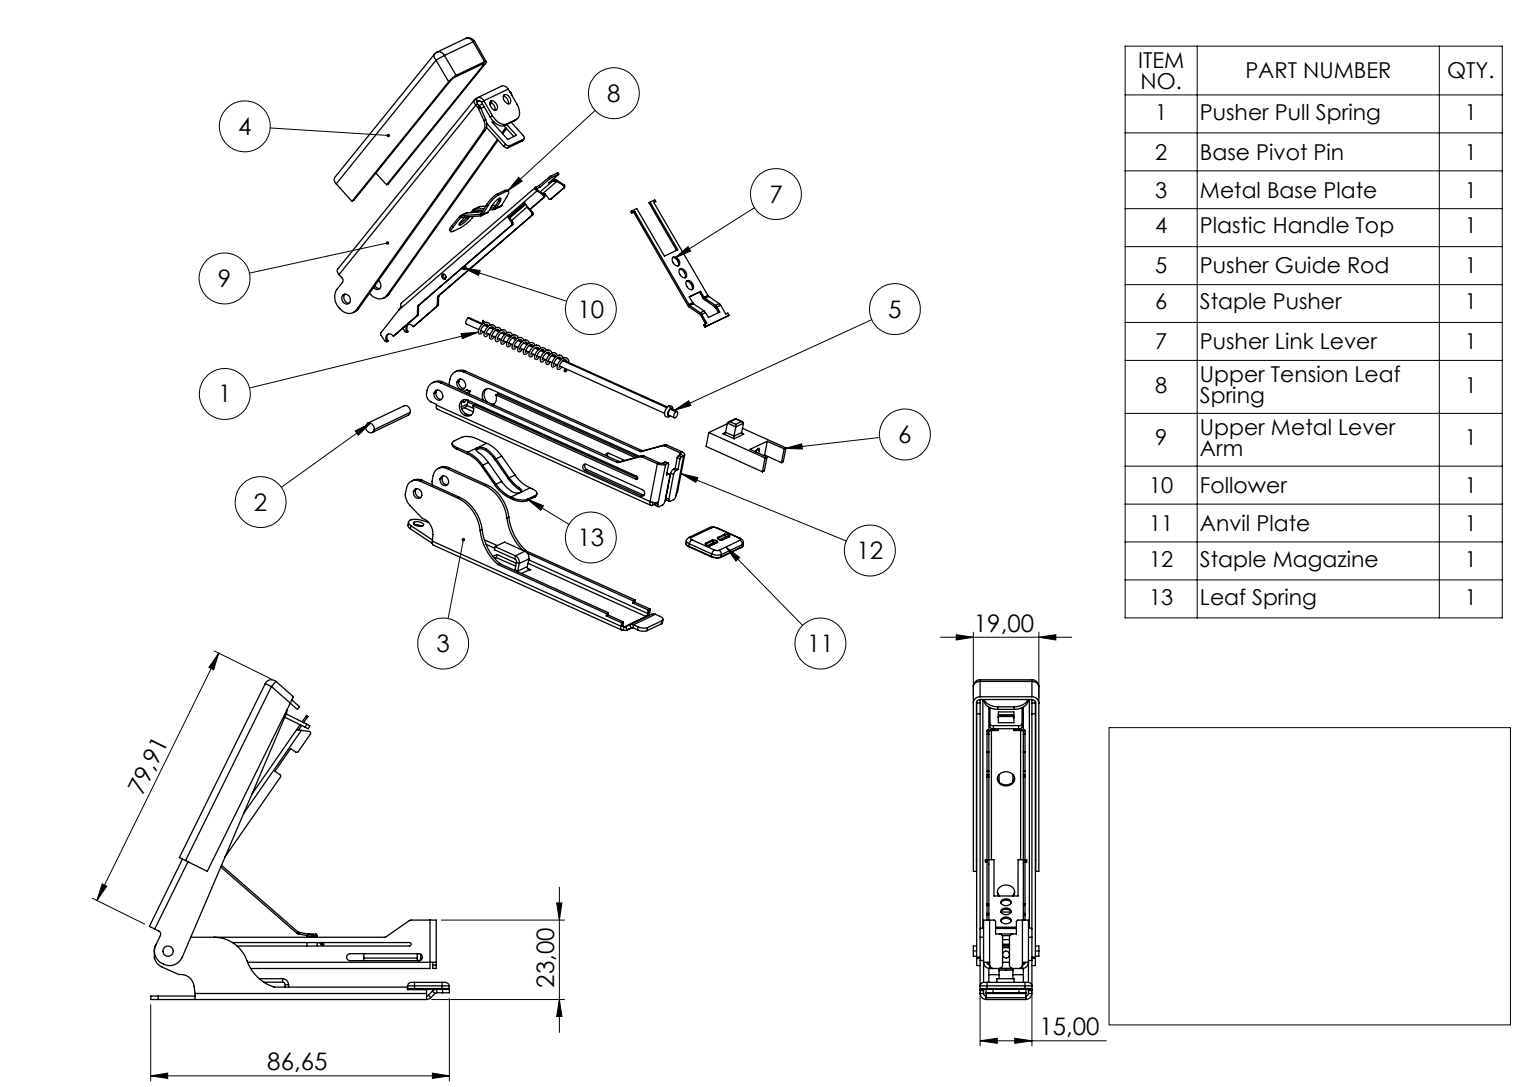
ISO-10303-21;
HEADER;
FILE_DESCRIPTION (('STEP AP214'),
    '1' );
FILE_NAME ('MAS-155',
    '2026-10-06T10:23:46',
    ( '' ),
    ( '' ),
    'SwSTEP 2.0',
    'SolidWorks 2020',
    '' );
FILE_SCHEMA (( 'AUTOMOTIVE_DESIGN' ));
ENDSEC;

DATA;
#1 = CARTESIAN_POINT ( 'NONE',  ( 35.64099152588522657, -0.6071811381869983704, 82.55501292736997243 ) ) ;
#2 = ORIENTED_EDGE ( 'NONE', *, *, #5924, .T. ) ;
#3 = DIRECTION ( 'NONE',  ( -2.412663730047099099E-15, 0.8967398287344627850, 0.4425581086832399147 ) ) ;
#4 = CARTESIAN_POINT ( 'NONE',  ( 32.56606138205700773, 43.35512946304240245, 83.12823623207320622 ) ) ;
#5 = CARTESIAN_POINT ( 'NONE',  ( 39.02088643472237806, -8.703840866421918676, 73.73360434286902887 ) ) ;
#6 = DIRECTION ( 'NONE',  ( 0.000000000000000000, 0.9992330079037401447, -0.03915859951075795903 ) ) ;
#7 = CARTESIAN_POINT ( 'NONE',  ( 38.82593461698262871, -16.91368208888610170, 69.62690120949091011 ) ) ;
#8 = FACE_OUTER_BOUND ( 'NONE', #24823, .T. ) ;
#9 = CARTESIAN_POINT ( 'NONE',  ( 37.25202387243752611, -25.21368208888610241, 70.00779233799262613 ) ) ;
#10 = VECTOR ( 'NONE', #20731, 1000.000000000000000 ) ;
#11 = DIRECTION ( 'NONE',  ( -6.056754644426120895E-31, -1.000000000000000000, -4.914813388431354887E-16 ) ) ;
#12 = CARTESIAN_POINT ( 'NONE',  ( 36.80608444377002542, -2.303840866421914768, 72.40698646996135324 ) ) ;
#13 = EDGE_CURVE ( 'NONE', #2345, #1520, #288, .T. ) ;
#14 = DIRECTION ( 'NONE',  ( 0.000000000000000000, 0.000000000000000000, 1.000000000000000000 ) ) ;
#15 = CARTESIAN_POINT ( 'NONE',  ( 39.82603832034400426, -20.31368208888610738, 72.40698646996133903 ) ) ;
#16 = EDGE_CURVE ( 'NONE', #3263, #15554, #24734, .T. ) ;
#17 = DIRECTION ( 'NONE',  ( -9.925461516413211857E-16, 0.8967398287344598984, 0.4425581086832454658 ) ) ;
#18 = CARTESIAN_POINT ( 'NONE',  ( 36.68196826583682935, -18.00384086642191406, 70.79240656858107172 ) ) ;
#19 = CARTESIAN_POINT ( 'NONE',  ( 35.14099152588522657, 1.392818861812999964, 83.30501292736997243 ) ) ;
#20 = CIRCLE ( 'NONE', #15263, 1.000000000000000888 ) ;
#21 = CARTESIAN_POINT ( 'NONE',  ( 36.64852494920107517, -13.41368208888610525, 70.89533451361947414 ) ) ;
#22 = VERTEX_POINT ( 'NONE', #10978 ) ;
#23 = CARTESIAN_POINT ( 'NONE',  ( 39.12911128074873801, -24.11368208888611164, 73.69843995877326392 ) ) ;
#24 = ORIENTED_EDGE ( 'NONE', *, *, #17686, .T. ) ;
#25 = DIRECTION ( 'NONE',  ( 8.673617379884039170E-17, 2.999999999999999839E-15, 1.000000000000000000 ) ) ;
#26 = DIRECTION ( 'NONE',  ( 1.327674326049719602E-15, -0.4425581086832399147, 0.8967398287344627850 ) ) ;
#27 = CIRCLE ( 'NONE', #15267, 0.2000000000000057288 ) ;
#28 = CARTESIAN_POINT ( 'NONE',  ( 38.26194895904384197, -26.60384086642191193, 72.51602215082114355 ) ) ;
#29 = EDGE_LOOP ( 'NONE', ( #453, #19107 ) ) ;
#30 = VERTEX_POINT ( 'NONE', #22566 ) ;
#31 = LINE ( 'NONE', #9973, #22803 ) ;
#32 = EDGE_CURVE ( 'NONE', #20252, #1331, #16766, .T. ) ;
#33 = CARTESIAN_POINT ( 'NONE',  ( 40.81606138205700773, -31.05876147765399864, 75.30501292737010033 ) ) ;
#34 = ORIENTED_EDGE ( 'NONE', *, *, #8349, .T. ) ;
#35 = DIRECTION ( 'NONE',  ( -1.000000000000000000, -3.091505625455828697E-15, -4.515976121274772923E-17 ) ) ;
#36 = CARTESIAN_POINT ( 'NONE',  ( 36.29569395875881099, -26.30384086642192187, 72.77780686321126780 ) ) ;
#37 = CARTESIAN_POINT ( 'NONE',  ( 33.31606138205700773, -26.06829118875199569, 75.80501292736998664 ) ) ;
#38 = CARTESIAN_POINT ( 'NONE',  ( 36.89935272106204422, -5.213682088886100630, 69.52238214136768590 ) ) ;
#39 = B_SPLINE_SURFACE_WITH_KNOTS ( 'NONE', 1, 3, ( 
 ( #3682, #6010, #7951, #7688 ),
 ( #11564, #15795, #4076, #7569 ) ),
 .UNSPECIFIED., .F., .F., .F.,
 ( 2, 2 ),
 ( 4, 4 ),
 ( 0.000000000000000000, 1.000000000000000000 ),
 ( 0.000000000000000000, 1.000000000000000000 ),
 .UNSPECIFIED. ) ;
#40 = CARTESIAN_POINT ( 'NONE',  ( 42.06606138205700063, 43.19123852234599781, 75.30501292736987295 ) ) ;
#41 = ORIENTED_EDGE ( 'NONE', *, *, #9883, .F. ) ;
#42 = ORIENTED_EDGE ( 'NONE', *, *, #4052, .T. ) ;
#43 = CARTESIAN_POINT ( 'NONE',  ( 33.24020206407681144, 3.104049617356281932, 6.135536031321588091 ) ) ;
#44 = CARTESIAN_POINT ( 'NONE',  ( 38.37017380507020192, 1.986317911113890444, 73.11602215082119471 ) ) ;
#45 = CARTESIAN_POINT ( 'NONE',  ( 36.80608444377002542, -24.30384086642191832, 72.40698646996131060 ) ) ;
#46 =( NAMED_UNIT ( * ) SI_UNIT ( $, .STERADIAN. ) SOLID_ANGLE_UNIT ( ) );
#47 = DIRECTION ( 'NONE',  ( 0.000000000000000000, 0.000000000000000000, -1.000000000000000000 ) ) ;
#48 = AXIS2_PLACEMENT_3D ( 'NONE', #18248, #195, #19789 ) ;
#49 = EDGE_LOOP ( 'NONE', ( #5787, #14617, #11097, #246 ) ) ;
#50 = DIRECTION ( 'NONE',  ( 1.000000000000000000, 2.751104698760144965E-15, -1.228345504986737969E-16 ) ) ;
#51 = VECTOR ( 'NONE', #12391, 1000.000000000000227 ) ;
#52 = CARTESIAN_POINT ( 'NONE',  ( 38.31606138205700773, -22.27515649656512053, 29.48506754039017963 ) ) ;
#53 = ORIENTED_EDGE ( 'NONE', *, *, #21241, .F. ) ;
#54 = CARTESIAN_POINT ( 'NONE',  ( 39.51027997493896748, -3.103840866421909706, 71.43714994484034264 ) ) ;
#55 = LINE ( 'NONE', #13982, #12355 ) ;
#56 = ORIENTED_EDGE ( 'NONE', *, *, #3919, .F. ) ;
#57 = DIRECTION ( 'NONE',  ( 0.000000000000000000, 1.000000000000000000, -3.469446951953613400E-15 ) ) ;
#58 = VERTEX_POINT ( 'NONE', #8676 ) ;
#59 = VERTEX_POINT ( 'NONE', #24601 ) ;
#60 = CARTESIAN_POINT ( 'NONE',  ( 41.31606138205700063, 9.119667998728431257, 66.98393923633439329 ) ) ;
#61 = CARTESIAN_POINT ( 'NONE',  ( 39.31564783533280405, -12.31368208888610027, 72.03616607671141026 ) ) ;
#62 = CARTESIAN_POINT ( 'NONE',  ( 39.51027997493896748, -10.51368208888610134, 71.32335560751961623 ) ) ;
#63 = ORIENTED_EDGE ( 'NONE', *, *, #7607, .F. ) ;
#64 = VERTEX_POINT ( 'NONE', #911 ) ;
#65 = DIRECTION ( 'NONE',  ( 0.000000000000000000, 1.000000000000000000, -2.775557561562891351E-15 ) ) ;
#66 = EDGE_CURVE ( 'NONE', #3119, #2388, #6890, .T. ) ;
#67 = CARTESIAN_POINT ( 'NONE',  ( 33.31606138205700773, -20.55619265724211076, 44.11584019928223910 ) ) ;
#68 = EDGE_LOOP ( 'NONE', ( #6538, #19929, #5268, #8723 ) ) ;
#69 = FACE_OUTER_BOUND ( 'NONE', #11931, .T. ) ;
#70 = CARTESIAN_POINT ( 'NONE',  ( 39.29254315202757653, -18.80384086642191477, 72.81632618279321889 ) ) ;
#71 = VECTOR ( 'NONE', #6423, 1000.000000000000227 ) ;
#72 = LINE ( 'NONE', #4208, #11613 ) ;
#73 = AXIS2_PLACEMENT_3D ( 'NONE', #20617, #20868, #18556 ) ;
#74 = DIRECTION ( 'NONE',  ( 0.000000000000000000, -0.5735764363510444941, 0.8191520442889929088 ) ) ;
#75 = CARTESIAN_POINT ( 'NONE',  ( 38.37017380507020192, -18.01368208888610312, 72.51602215082118619 ) ) ;
#76 = ORIENTED_EDGE ( 'NONE', *, *, #14029, .F. ) ;
#77 = ORIENTED_EDGE ( 'NONE', *, *, #24683, .F. ) ;
#78 = FACE_BOUND ( 'NONE', #23310, .T. ) ;
#79 = CARTESIAN_POINT ( 'NONE',  ( 37.33957961208646736, -13.81368208888610916, 72.81632618279321889 ) ) ;
#80 = CARTESIAN_POINT ( 'NONE',  ( 44.81606138205700063, -25.52563857111379875, 92.39878177866870601 ) ) ;
#81 = CARTESIAN_POINT ( 'NONE',  ( 43.81606138205700063, -33.39268736607245103, 60.15578379404454523 ) ) ;
#82 = CARTESIAN_POINT ( 'NONE',  ( 39.82603832034400426, -28.31368208888610027, 72.40698646996131060 ) ) ;
#83 = CARTESIAN_POINT ( 'NONE',  ( 40.08931077638955998, -29.10876147764802369, 70.44264307849509521 ) ) ;
#84 = CIRCLE ( 'NONE', #17364, 0.7500000000000006661 ) ;
#85 = CARTESIAN_POINT ( 'NONE',  ( 33.31606138205700773, -20.55619265724211076, 44.11584019928223910 ) ) ;
#86 = ORIENTED_EDGE ( 'NONE', *, *, #3104, .F. ) ;
#87 = VECTOR ( 'NONE', #691, 1000.000000000000114 ) ;
#88 = CARTESIAN_POINT ( 'NONE',  ( 33.31606138205700773, 7.043113989679085307, 66.83274420321491505 ) ) ;
#89 = EDGE_LOOP ( 'NONE', ( #3243, #17530, #4061, #10924 ) ) ;
#90 = ORIENTED_EDGE ( 'NONE', *, *, #479, .T. ) ;
#91 = CARTESIAN_POINT ( 'NONE',  ( 39.73277004305197124, -5.403840866421909972, 69.52238214136768590 ) ) ;
#92 = ORIENTED_EDGE ( 'NONE', *, *, #24380, .T. ) ;
#93 = AXIS2_PLACEMENT_3D ( 'NONE', #14032, #16324, #20207 ) ;
#94 = EDGE_CURVE ( 'NONE', #4444, #1424, #20510, .T. ) ;
#95 = DIRECTION ( 'NONE',  ( 1.000000000000000000, 0.000000000000000000, 0.000000000000000000 ) ) ;
#96 = CARTESIAN_POINT ( 'NONE',  ( 39.95015449827720744, -8.613682088886104538, 70.79240656858107172 ) ) ;
#97 = EDGE_LOOP ( 'NONE', ( #25397, #5551, #19425, #6383 ) ) ;
#98 = CARTESIAN_POINT ( 'NONE',  ( 29.81606138205697221, -3.227578639999851617, -4.500312080287595329 ) ) ;
#99 = CARTESIAN_POINT ( 'NONE',  ( 40.33642880535524000, -12.31368208888611093, 72.77780686321126780 ) ) ;
#100 = DIRECTION ( 'NONE',  ( 0.000000000000000000, -0.5706330172266907974, 0.8212051873014217795 ) ) ;
#101 = CARTESIAN_POINT ( 'NONE',  ( 35.64099152588522657, 40.83281886181300280, 79.30501292736983032 ) ) ;
#102 = AXIS2_PLACEMENT_3D ( 'NONE', #15158, #5376, #18644 ) ;
#103 = DIRECTION ( 'NONE',  ( 2.312964634635740294E-15, 2.999999999999999839E-15, 1.000000000000000000 ) ) ;
#104 = ADVANCED_FACE ( 'NONE', ( #4789 ), #24864, .T. ) ;
#105 =( NAMED_UNIT ( * ) PLANE_ANGLE_UNIT ( ) SI_UNIT ( $, .RADIAN. ) );
#106 = ADVANCED_FACE ( 'NONE', ( #10603 ), #18707, .F. ) ;
#107 = LINE ( 'NONE', #13782, #2826 ) ;
#108 = VECTOR ( 'NONE', #19668, 1000.000000000000000 ) ;
#109 = EDGE_CURVE ( 'NONE', #2100, #16742, #24351, .T. ) ;
#110 = LINE ( 'NONE', #17914, #18667 ) ;
#111 = EDGE_CURVE ( 'NONE', #24693, #6631, #6848, .T. ) ;
#112 = CARTESIAN_POINT ( 'NONE',  ( 37.69225076346193504, -15.80384086642191299, 70.42958956619168021 ) ) ;
#113 = CARTESIAN_POINT ( 'NONE',  ( 39.37952058850012804, -22.61368208888610454, 70.97781676520601479 ) ) ;
#114 = EDGE_CURVE ( 'NONE', #23891, #14933, #22516, .T. ) ;
#115 = ORIENTED_EDGE ( 'NONE', *, *, #16759, .F. ) ;
#116 = CARTESIAN_POINT ( 'NONE',  ( 44.81606138205700063, -24.55876147765401285, 70.30501292737008612 ) ) ;
#117 = VECTOR ( 'NONE', #18081, 1000.000000000000000 ) ;
#118 = CYLINDRICAL_SURFACE ( 'NONE', #9476, 1.000000000000000888 ) ;
#119 = ORIENTED_EDGE ( 'NONE', *, *, #11030, .T. ) ;
#120 = VERTEX_POINT ( 'NONE', #3105 ) ;
#121 = CARTESIAN_POINT ( 'NONE',  ( 38.26194895904384197, -22.60384086642191903, 73.71602215082113219 ) ) ;
#122 = AXIS2_PLACEMENT_3D ( 'NONE', #22603, #19127, #1077 ) ;
#123 = ADVANCED_FACE ( 'NONE', ( #785 ), #7110, .F. ) ;
#124 = CARTESIAN_POINT ( 'NONE',  ( 37.12184278917507640, -23.51368208888609956, 71.43714994484032843 ) ) ;
#125 = CARTESIAN_POINT ( 'NONE',  ( 37.61123632939165873, -5.913682088886105248, 73.73360434286902887 ) ) ;
#126 = VERTEX_POINT ( 'NONE', #6729 ) ;
#127 = DIRECTION ( 'NONE',  ( 0.000000000000000000, 1.000000000000000000, -2.775557561562891351E-15 ) ) ;
#128 = EDGE_CURVE ( 'NONE', #1147, #21871, #2352, .T. ) ;
#129 = CARTESIAN_POINT ( 'NONE',  ( 37.25260217561390874, -0.003840866421911393481, 70.97781676520604321 ) ) ;
#130 = FACE_OUTER_BOUND ( 'NONE', #3742, .T. ) ;
#131 = VERTEX_POINT ( 'NONE', #14581 ) ;
#132 = AXIS2_PLACEMENT_3D ( 'NONE', #6490, #16519, #18844 ) ;
#133 = CARTESIAN_POINT ( 'NONE',  ( 40.64099152588522657, -1.357181138186998925, 80.05501292737000085 ) ) ;
#134 = DIRECTION ( 'NONE',  ( 0.000000000000000000, -0.8212051873014223347, -0.5706330172266899092 ) ) ;
#135 = CARTESIAN_POINT ( 'NONE',  ( 36.89935272106205133, -6.403840866421917077, 73.23812341099225875 ) ) ;
#136 = FACE_OUTER_BOUND ( 'NONE', #6898, .T. ) ;
#137 = SURFACE_STYLE_USAGE ( .BOTH. , #13306 ) ;
#138 = MECHANICAL_DESIGN_GEOMETRIC_PRESENTATION_REPRESENTATION (  '', ( #5078 ), #1784 ) ;
#139 = CARTESIAN_POINT ( 'NONE',  ( 39.95015449827720744, -12.61368208888610454, 70.79240656858105751 ) ) ;
#140 = CARTESIAN_POINT ( 'NONE',  ( 33.63257508155574271, 2.837830513113388076, 6.099065269017614810 ) ) ;
#141 = EDGE_CURVE ( 'NONE', #14226, #13391, #3231, .T. ) ;
#142 = CARTESIAN_POINT ( 'NONE',  ( 36.87297107704153376, -25.71368208888610596, 72.49904802271738902 ) ) ;
#143 = VECTOR ( 'NONE', #19074, 1000.000000000000000 ) ;
#144 = LINE ( 'NONE', #15861, #20989 ) ;
#145 = CIRCLE ( 'NONE', #6320, 1.000000000000000888 ) ;
#146 = CARTESIAN_POINT ( 'NONE',  ( 36.87297107704151244, -1.903840866421906641, 70.26145752964255564 ) ) ;
#147 = CARTESIAN_POINT ( 'NONE',  ( 38.48938833801555148, 40.69123852234599781, 72.28987726642291989 ) ) ;
#148 = CARTESIAN_POINT ( 'NONE',  ( 36.80608444377001121, -19.31368208888609672, 70.35351908239857721 ) ) ;
#149 = DIRECTION ( 'NONE',  ( 0.000000000000000000, -0.7540134720837687876, -0.6568589528324780824 ) ) ;
#150 = AXIS2_PLACEMENT_3D ( 'NONE', #11257, #7991, #1314 ) ;
#151 = CARTESIAN_POINT ( 'NONE',  ( 39.38009889167648936, -17.40384086642190908, 70.00779233799262613 ) ) ;
#152 = LINE ( 'NONE', #3900, #22918 ) ;
#153 = CARTESIAN_POINT ( 'NONE',  ( 36.64852494920107517, -11.41368208888610525, 70.89533451361947414 ) ) ;
#154 = VERTEX_POINT ( 'NONE', #12549 ) ;
#155 = CARTESIAN_POINT ( 'NONE',  ( 37.50301148336529167, -19.11368208888609388, 69.06206559358665231 ) ) ;
#156 = ORIENTED_EDGE ( 'NONE', *, *, #18156, .F. ) ;
#157 = CARTESIAN_POINT ( 'NONE',  ( 36.31606138205700063, 39.69123852234597649, 69.30501292736988717 ) ) ;
#158 = AXIS2_PLACEMENT_3D ( 'NONE', #16213, #10429, #24064 ) ;
#159 = CARTESIAN_POINT ( 'NONE',  ( 41.31606138205700063, 7.187001342539796944, 66.09667597968754649 ) ) ;
#160 = CARTESIAN_POINT ( 'NONE',  ( 38.73920764526923932, -19.50384086642191406, 70.26206559358661252 ) ) ;
#161 = ORIENTED_EDGE ( 'NONE', *, *, #12871, .T. ) ;
#162 = ORIENTED_EDGE ( 'NONE', *, *, #2908, .T. ) ;
#163 = CARTESIAN_POINT ( 'NONE',  ( 39.59824383043523000, -28.76838690529542220, 70.55371702292011094 ) ) ;
#164 = CIRCLE ( 'NONE', #21962, 1.000000000000000888 ) ;
#165 = LINE ( 'NONE', #13580, #21925 ) ;
#166 = CARTESIAN_POINT ( 'NONE',  ( 40.26954217208372455, -20.90384086642191974, 72.86986841596734621 ) ) ;
#167 = CARTESIAN_POINT ( 'NONE',  ( 36.07789103942398867, 0.5863179111138955291, 70.70992431699450265 ) ) ;
#168 = DIRECTION ( 'NONE',  ( 0.000000000000000000, 1.000000000000000000, -3.469446951953613400E-15 ) ) ;
#169 = ORIENTED_EDGE ( 'NONE', *, *, #3276, .T. ) ;
#170 = VERTEX_POINT ( 'NONE', #12668 ) ;
#171 = CARTESIAN_POINT ( 'NONE',  ( 43.31606138205700063, 3.536347952325769040, 64.10938348997790115 ) ) ;
#172 =( GEOMETRIC_REPRESENTATION_CONTEXT ( 3 ) GLOBAL_UNCERTAINTY_ASSIGNED_CONTEXT ( ( #8249 ) ) GLOBAL_UNIT_ASSIGNED_CONTEXT ( ( #2358, #16143, #22073 ) ) REPRESENTATION_CONTEXT ( 'NONE', 'WORKASPACE' ) );
#173 = DIRECTION ( 'NONE',  ( 0.000000000000000000, 1.000000000000000000, -3.469446951953701358E-15 ) ) ;
#174 = CARTESIAN_POINT ( 'NONE',  ( 36.68196826583682935, -24.00384086642191050, 70.79240656858105751 ) ) ;
#175 = FILL_AREA_STYLE ('',( #23869 ) ) ;
#176 = DIRECTION ( 'NONE',  ( 0.000000000000000000, 0.9814242980364923374, 0.1918498038142812112 ) ) ;
#177 = ORIENTED_EDGE ( 'NONE', *, *, #13046, .F. ) ;
#178 = LINE ( 'NONE', #16145, #1575 ) ;
#179 = DIRECTION ( 'NONE',  ( 1.000000000000000000, -5.204170427930413997E-31, -1.734723475976804876E-16 ) ) ;
#180 = VERTEX_POINT ( 'NONE', #7626 ) ;
#181 = CARTESIAN_POINT ( 'NONE',  ( 39.41296390513587511, -9.203840866421909794, 71.08074471024443142 ) ) ;
#182 = CARTESIAN_POINT ( 'NONE',  ( 42.90896497783001706, 3.030042170879425178, 6.235548050178295831 ) ) ;
#183 = ORIENTED_EDGE ( 'NONE', *, *, #6628, .F. ) ;
#184 = CARTESIAN_POINT ( 'NONE',  ( 31.91606138205697718, -5.022037326221728826, -5.474317061061731771 ) ) ;
#185 = ORIENTED_EDGE ( 'NONE', *, *, #16638, .F. ) ;
#186 = ORIENTED_EDGE ( 'NONE', *, *, #12634, .T. ) ;
#187 = CARTESIAN_POINT ( 'NONE',  ( 43.23147868389327897, 41.90149715599300606, 79.87823623207322044 ) ) ;
#188 = CARTESIAN_POINT ( 'NONE',  ( 39.31564783533280405, -6.313682088886101162, 72.03616607671141026 ) ) ;
#189 = CARTESIAN_POINT ( 'NONE',  ( 39.02742774030102879, -4.213682088886099741, 72.26730301774236409 ) ) ;
#190 = ORIENTED_EDGE ( 'NONE', *, *, #18404, .F. ) ;
#191 = EDGE_LOOP ( 'NONE', ( #11726, #12081, #22272, #24674 ) ) ;
#192 = DIRECTION ( 'NONE',  ( 0.000000000000000000, 1.000000000000000000, -3.469446951953613400E-15 ) ) ;
#193 = DIRECTION ( 'NONE',  ( -1.927470528863119788E-16, -1.000000000000000000, 2.999999999999999839E-15 ) ) ;
#194 = VERTEX_POINT ( 'NONE', #1 ) ;
#195 = DIRECTION ( 'NONE',  ( 1.000000000000000000, -0.000000000000000000, 0.000000000000000000 ) ) ;
#196 = CARTESIAN_POINT ( 'NONE',  ( 38.93415946300896024, -17.50384086642190695, 69.66206559358661821 ) ) ;
#197 = VECTOR ( 'NONE', #7883, 1000.000000000000000 ) ;
#198 = EDGE_CURVE ( 'NONE', #24709, #13605, #5816, .T. ) ;
#199 = EDGE_CURVE ( 'NONE', #8460, #24765, #19336, .T. ) ;
#200 = CARTESIAN_POINT ( 'NONE',  ( 37.42719827050449055, -22.02795882147844964, 75.81186121921504650 ) ) ;
#201 = CARTESIAN_POINT ( 'NONE',  ( 44.81606138205700063, 41.44123852234595518, 61.30501292736988006 ) ) ;
#202 = CARTESIAN_POINT ( 'NONE',  ( 44.81606138205700063, 40.34464305740947765, 81.44836866983821722 ) ) ;
#203 = VERTEX_POINT ( 'NONE', #23192 ) ;
#204 = ORIENTED_EDGE ( 'NONE', *, *, #17940, .F. ) ;
#205 = LINE ( 'NONE', #24148, #14945 ) ;
#206 = CARTESIAN_POINT ( 'NONE',  ( 39.82603832034401847, -12.31368208888610738, 72.40698646996131060 ) ) ;
#207 = CARTESIAN_POINT ( 'NONE',  ( 40.31606138205700773, 37.94123852234599070, 73.55501292736988717 ) ) ;
#208 = LINE ( 'NONE', #4092, #1342 ) ;
#209 = LINE ( 'NONE', #23668, #17662 ) ;
#210 = LINE ( 'NONE', #8213, #17640 ) ;
#211 = ADVANCED_FACE ( 'NONE', ( #19460 ), #5431, .T. ) ;
#212 = VECTOR ( 'NONE', #20996, 1000.000000000000000 ) ;
#213 = AXIS2_PLACEMENT_3D ( 'NONE', #12528, #8134, #2696 ) ;
#214 = CARTESIAN_POINT ( 'NONE',  ( 33.31606138205700773, -14.32738121993777192, 11.12118157620986558 ) ) ;
#215 = LINE ( 'NONE', #15932, #731 ) ;
#216 = EDGE_LOOP ( 'NONE', ( #18034, #25103, #6817, #21837 ) ) ;
#217 = CARTESIAN_POINT ( 'NONE',  ( 31.81606138205700418, -31.45856502260510013, 77.07494475056050476 ) ) ;
#218 = EDGE_LOOP ( 'NONE', ( #9842, #8008, #1464, #22702 ) ) ;
#219 = ORIENTED_EDGE ( 'NONE', *, *, #5616, .T. ) ;
#220 = CARTESIAN_POINT ( 'NONE',  ( 36.11133435605973574, -6.003840866421917610, 70.60699637195612866 ) ) ;
#221 = ORIENTED_EDGE ( 'NONE', *, *, #10919, .F. ) ;
#222 = DIRECTION ( 'NONE',  ( 0.000000000000000000, -2.999999999999999839E-15, -1.000000000000000000 ) ) ;
#223 = CARTESIAN_POINT ( 'NONE',  ( 37.80618814713140097, -9.913682088886107024, 73.13360434286904876 ) ) ;
#224 = ORIENTED_EDGE ( 'NONE', *, *, #10845, .T. ) ;
#225 = CARTESIAN_POINT ( 'NONE',  ( 30.81606138205700418, -21.15876147765410309, 66.30501292737000085 ) ) ;
#226 = CARTESIAN_POINT ( 'NONE',  ( 36.29569395875879678, -15.31368208888610205, 69.98269868914867686 ) ) ;
#227 = DIRECTION ( 'NONE',  ( -1.000000000000000000, -2.999999999999999839E-15, 0.000000000000000000 ) ) ;
#228 = CARTESIAN_POINT ( 'NONE',  ( 32.81606138205700773, 36.92314894770294131, 81.17823623207323180 ) ) ;
#229 = CYLINDRICAL_SURFACE ( 'NONE', #16961, 0.5000000000000004441 ) ;
#230 = DIRECTION ( 'NONE',  ( 1.000000000000000000, 1.518641380243644581E-16, 1.055262346480601087E-16 ) ) ;
#231 = EDGE_CURVE ( 'NONE', #16465, #14577, #22942, .T. ) ;
#232 = CARTESIAN_POINT ( 'NONE',  ( 32.81606138205700773, -27.11289203277224402, 56.96090842897168471 ) ) ;
#233 = DIRECTION ( 'NONE',  ( -1.849283715844614702E-16, 0.8212051873014210024, 0.5706330172266920187 ) ) ;
#234 = CARTESIAN_POINT ( 'NONE',  ( 38.93987200065208754, -24.81368208888610738, 70.42958956619166599 ) ) ;
#235 = VERTEX_POINT ( 'NONE', #24984 ) ;
#236 = CARTESIAN_POINT ( 'NONE',  ( 40.81606138205700063, 9.191238522346999673, 69.30501292736997243 ) ) ;
#237 = DIRECTION ( 'NONE',  ( 1.000000000000000000, 0.000000000000000000, 0.000000000000000000 ) ) ;
#238 = ORIENTED_EDGE ( 'NONE', *, *, #7921, .F. ) ;
#239 = ORIENTED_EDGE ( 'NONE', *, *, #12746, .F. ) ;
#240 = CARTESIAN_POINT ( 'NONE',  ( 37.61123632939164452, -25.70384086642191690, 69.02690120949091579 ) ) ;
#241 = CARTESIAN_POINT ( 'NONE',  ( 37.33957961208646736, -27.81368208888611093, 72.81632618279320468 ) ) ;
#242 = DIRECTION ( 'NONE',  ( 1.218693434051482139E-16, -0.4425581086832393041, 0.8967398287344630070 ) ) ;
#243 = EDGE_CURVE ( 'NONE', #17020, #9362, #11367, .T. ) ;
#244 = LINE ( 'NONE', #4267, #5670 ) ;
#245 = EDGE_CURVE ( 'NONE', #15791, #17958, #9316, .T. ) ;
#246 = ORIENTED_EDGE ( 'NONE', *, *, #17263, .T. ) ;
#247 = CARTESIAN_POINT ( 'NONE',  ( 39.93368021267864520, -5.986475166052370511, 82.77450256188085120 ) ) ;
#248 = CYLINDRICAL_SURFACE ( 'NONE', #25213, 0.7500000000000006661 ) ;
#249 = CARTESIAN_POINT ( 'NONE',  ( 40.77203464402485622, -1.103840866421915035, 71.43714994484034264 ) ) ;
#250 = EDGE_CURVE ( 'NONE', #6034, #3058, #21270, .T. ) ;
#251 = EDGE_CURVE ( 'NONE', #21293, #8440, #21528, .T. ) ;
#252 = ADVANCED_FACE ( 'NONE', ( #23316 ), #17669, .F. ) ;
#253 = DIRECTION ( 'NONE',  ( 1.000000000000000275E-15, -0.9439899321577401858, -0.3299742535180970604 ) ) ;
#254 = CYLINDRICAL_SURFACE ( 'NONE', #13248, 1.000000000000000888 ) ;
#255 = CARTESIAN_POINT ( 'NONE',  ( 39.95015449827720744, -4.613682088886104538, 70.79240656858107172 ) ) ;
#256 = CARTESIAN_POINT ( 'NONE',  ( 39.29254315202756231, -24.81368208888610383, 69.94417936956671156 ) ) ;
#257 = CARTESIAN_POINT ( 'NONE',  ( 34.56606138205700773, 45.04446929126255128, 81.37823623207320622 ) ) ;
#258 = ADVANCED_FACE ( 'NONE', ( #25369 ), #5308, .T. ) ;
#259 = CARTESIAN_POINT ( 'NONE',  ( 39.98359781491296161, -3.203840866421912903, 70.89533451361947414 ) ) ;
#261 = EDGE_CURVE ( 'NONE', #11274, #17540, #5561, .T. ) ;
#260 = CONTEXT_DEPENDENT_SHAPE_REPRESENTATION ( #7838, #3099 ) ;
#262 = CARTESIAN_POINT ( 'NONE',  ( 32.81606138205700773, 2.191238522347013440, 73.80501292737000085 ) ) ;
#263 = CARTESIAN_POINT ( 'NONE',  ( 37.21915885897815457, -26.20384086642190979, 71.67976084211551324 ) ) ;
#264 = CARTESIAN_POINT ( 'NONE',  ( 36.64852494920107517, -9.413682088886107024, 70.89533451361948835 ) ) ;
#265 = LINE ( 'NONE', #13690, #19298 ) ;
#266 = AXIS2_PLACEMENT_3D ( 'NONE', #24025, #20423, #700 ) ;
#267 = CARTESIAN_POINT ( 'NONE',  ( 36.64852494920107517, -10.20384086642191157, 71.86517103874049894 ) ) ;
#268 = DIRECTION ( 'NONE',  ( 1.000000000000000000, 3.083952846180988900E-15, -3.854941057726327830E-16 ) ) ;
#269 = VECTOR ( 'NONE', #16270, 1000.000000000000000 ) ;
#270 = CIRCLE ( 'NONE', #24538, 2.000000000000001776 ) ;
#271 = CARTESIAN_POINT ( 'NONE',  ( 36.64852494920107517, -9.413682088886107024, 70.89533451361948835 ) ) ;
#272 = ORIENTED_EDGE ( 'NONE', *, *, #16077, .F. ) ;
#273 = CARTESIAN_POINT ( 'NONE',  ( 38.37017380507020192, -18.01368208888610667, 73.71602215082113219 ) ) ;
#274 = EDGE_LOOP ( 'NONE', ( #318, #14239, #23744, #24928 ) ) ;
#275 = DIRECTION ( 'NONE',  ( -1.000000000000000000, -1.734723475976799945E-16, 1.734723475976814737E-16 ) ) ;
#276 = CARTESIAN_POINT ( 'NONE',  ( 33.31606138205700773, -21.26162886970023536, 44.16441745890789150 ) ) ;
#277 = CARTESIAN_POINT ( 'NONE',  ( 38.63098279924290068, -16.70384086642190624, 72.53360434286904024 ) ) ;
#278 = ORIENTED_EDGE ( 'NONE', *, *, #24831, .T. ) ;
#279 = ORIENTED_EDGE ( 'NONE', *, *, #5950, .F. ) ;
#280 = CARTESIAN_POINT ( 'NONE',  ( 30.81606138205700418, -0.6071811381869983704, 82.55501292736998664 ) ) ;
#281 = DIRECTION ( 'NONE',  ( 1.000000000000000000, 1.187136597504755470E-16, 8.249087426255173666E-17 ) ) ;
#282 = CARTESIAN_POINT ( 'NONE',  ( 37.61123632939164452, -19.70384086642190979, 69.02690120949091579 ) ) ;
#283 = ADVANCED_FACE ( 'NONE', ( #13171 ), #7751, .T. ) ;
#284 = EDGE_CURVE ( 'NONE', #21429, #18272, #15214, .T. ) ;
#285 = CARTESIAN_POINT ( 'NONE',  ( 44.81606138205700063, -34.55876147765400930, 73.30501292737011454 ) ) ;
#286 = CARTESIAN_POINT ( 'NONE',  ( 39.82603832034400426, -26.31368208888611093, 72.40698646996131060 ) ) ;
#287 = LINE ( 'NONE', #10351, #18422 ) ;
#288 = CIRCLE ( 'NONE', #14300, 0.7106531558045068309 ) ;
#289 = ORIENTED_EDGE ( 'NONE', *, *, #17382, .F. ) ;
#290 = ORIENTED_EDGE ( 'NONE', *, *, #14159, .F. ) ;
#291 = VECTOR ( 'NONE', #3755, 1000.000000000000000 ) ;
#292 = VECTOR ( 'NONE', #25323, 1000.000000000000000 ) ;
#293 = CARTESIAN_POINT ( 'NONE',  ( 40.31606138205700773, 39.69123852234597649, 69.30501292736988717 ) ) ;
#294 = DIRECTION ( 'NONE',  ( 0.000000000000000000, 2.775557561562888984E-15, 1.000000000000000000 ) ) ;
#295 = B_SPLINE_CURVE_WITH_KNOTS ( 'NONE', 3,
 ( #12547, #1271, #23035, #14456, #20383, #15309, #9152 ),
 .UNSPECIFIED., .F., .F.,
 ( 4, 3, 4 ),
 ( 0.000000000000000000, 0.9999934796777874002, 1.000000000000000000 ),
 .UNSPECIFIED. ) ;
#296 = CARTESIAN_POINT ( 'NONE',  ( 39.29254315202757653, -20.80384086642191832, 72.81632618279321889 ) ) ;
#297 = DIRECTION ( 'NONE',  ( 0.000000000000000000, -2.999999999999999839E-15, -1.000000000000000000 ) ) ;
#298 = ORIENTED_EDGE ( 'NONE', *, *, #19568, .F. ) ;
#299 = LINE ( 'NONE', #10238, #21343 ) ;
#300 = DIRECTION ( 'NONE',  ( 0.000000000000000000, -0.8212051873014210024, -0.5706330172266920187 ) ) ;
#301 = CARTESIAN_POINT ( 'NONE',  ( 38.26194895904384197, -0.6038408664219111488, 72.51602215082118619 ) ) ;
#302 = FACE_OUTER_BOUND ( 'NONE', #11083, .T. ) ;
#303 = ORIENTED_EDGE ( 'NONE', *, *, #10224, .F. ) ;
#304 = ADVANCED_FACE ( 'NONE', ( #3366 ), #21151, .F. ) ;
#305 = CARTESIAN_POINT ( 'NONE',  ( -3.469446951953610245E-16, 2.753545109730417678E-13, 79.37823623207336254 ) ) ;
#306 = ORIENTED_EDGE ( 'NONE', *, *, #2685, .F. ) ;
#307 = ORIENTED_EDGE ( 'NONE', *, *, #22779, .T. ) ;
#308 = VECTOR ( 'NONE', #6285, 1000.000000000000000 ) ;
#309 = CARTESIAN_POINT ( 'NONE',  ( 37.14448850680319225, -21.82678658219787948, 29.70634659473178374 ) ) ;
#310 = DIRECTION ( 'NONE',  ( 1.000000000000000000, 0.000000000000000000, 0.000000000000000000 ) ) ;
#311 = CARTESIAN_POINT ( 'NONE',  ( 37.38336156205274818, -5.713682088886101518, 72.12822762946751709 ) ) ;
#312 = VECTOR ( 'NONE', #16987, 1000.000000000000000 ) ;
#313 = CARTESIAN_POINT ( 'NONE',  ( 39.02742774030102879, -6.213682088886101518, 72.26730301774236409 ) ) ;
#314 = ORIENTED_EDGE ( 'NONE', *, *, #23269, .F. ) ;
#315 = ORIENTED_EDGE ( 'NONE', *, *, #21706, .T. ) ;
#316 = CARTESIAN_POINT ( 'NONE',  ( 40.31606138205700773, 38.69123852234599070, 73.55501292736988717 ) ) ;
#317 = CARTESIAN_POINT ( 'NONE',  ( 31.81606138205700418, -24.55876147765401285, 70.30501292737008612 ) ) ;
#318 = ORIENTED_EDGE ( 'NONE', *, *, #8973, .F. ) ;
#319 = CYLINDRICAL_SURFACE ( 'NONE', #22266, 1.000000000000000888 ) ;
#320 = CARTESIAN_POINT ( 'NONE',  ( 37.33957961208645315, -9.803840866421907663, 69.94417936956673998 ) ) ;
#321 = CARTESIAN_POINT ( 'NONE',  ( 36.37840728046802496, -20.80847383641847870, 75.91491741683218208 ) ) ;
#322 = MANIFOLD_SOLID_BREP ( 'NONE', #22112 ) ;
#323 = LINE ( 'NONE', #12708, #17156 ) ;
#324 = ORIENTED_EDGE ( 'NONE', *, *, #10135, .F. ) ;
#325 = ORIENTED_EDGE ( 'NONE', *, *, #16629, .F. ) ;
#326 = CARTESIAN_POINT ( 'NONE',  ( 42.82259893474252266, 3.224890024296139135, 6.370941811568299862 ) ) ;
#327 = CARTESIAN_POINT ( 'NONE',  ( 37.69796330110504101, -7.113682088886101873, 69.66206559358664663 ) ) ;
#328 = CARTESIAN_POINT ( 'NONE',  ( 31.81606138205700418, 28.69846577177642288, 66.12638289304319983 ) ) ;
#329 = CARTESIAN_POINT ( 'NONE',  ( 31.81606138205700418, 44.92314894770293421, 79.37823623207320622 ) ) ;
#330 = CIRCLE ( 'NONE', #7350, 1.500000000000001332 ) ;
#331 = LINE ( 'NONE', #20056, #8211 ) ;
#332 = DIRECTION ( 'NONE',  ( 1.734723475976814737E-16, -1.000000000000000000, 3.491481338843135327E-15 ) ) ;
#333 = EDGE_CURVE ( 'NONE', #14933, #7242, #7489, .T. ) ;
#334 = DIRECTION ( 'NONE',  ( -1.000000000000000000, 0.000000000000000000, 0.000000000000000000 ) ) ;
#335 = PLANE ( 'NONE',  #18029 ) ;
#336 = EDGE_CURVE ( 'NONE', #3808, #21524, #7738, .T. ) ;
#337 = CARTESIAN_POINT ( 'NONE',  ( 32.56606138205700773, 40.39281886181299797, 83.30501292736984453 ) ) ;
#338 = ORIENTED_EDGE ( 'NONE', *, *, #17984, .T. ) ;
#339 = EDGE_LOOP ( 'NONE', ( #14146, #23745, #1697, #21573 ) ) ;
#340 = CARTESIAN_POINT ( 'NONE',  ( 35.81606138205700063, -6.549308025893449070, 20.35783565644092619 ) ) ;
#341 = CARTESIAN_POINT ( 'NONE',  ( 35.86008812008917346, -6.103840866421916367, 71.32335560751961623 ) ) ;
#342 = ORIENTED_EDGE ( 'NONE', *, *, #16102, .F. ) ;
#343 = CARTESIAN_POINT ( 'NONE',  ( 45.81606138205698642, -7.197381196808444237, -3.552044091124070491 ) ) ;
#344 = CARTESIAN_POINT ( 'NONE',  ( 39.98359781491296161, -6.413682088886103472, 71.86517103874048473 ) ) ;
#345 = VECTOR ( 'NONE', #23044, 1000.000000000000000 ) ;
#346 = EDGE_LOOP ( 'NONE', ( #3037, #6134, #10339, #6691 ) ) ;
#347 = DIRECTION ( 'NONE',  ( -3.717264591378870232E-16, -3.325260651745651169E-15, -1.000000000000000000 ) ) ;
#348 = EDGE_CURVE ( 'NONE', #23547, #5555, #499, .T. ) ;
#349 = CARTESIAN_POINT ( 'NONE',  ( 39.12911128074873801, -16.11368208888610809, 73.69843995877327814 ) ) ;
#350 = CARTESIAN_POINT ( 'NONE',  ( 42.98956905832248765, 3.335839619497401376, 6.349669990345183201 ) ) ;
#351 = FACE_OUTER_BOUND ( 'NONE', #1891, .T. ) ;
#352 = CARTESIAN_POINT ( 'NONE',  ( 33.40064408022072939, 41.90149715599300606, 79.37823623207322044 ) ) ;
#353 = VECTOR ( 'NONE', #14172, 1000.000000000000000 ) ;
#354 = DIRECTION ( 'NONE',  ( -0.6683808861234329379, -0.6108281792586462977, -0.4244477900618892630 ) ) ;
#355 = CARTESIAN_POINT ( 'NONE',  ( 33.56606138205700773, 41.44123852234599070, 73.55501292736987295 ) ) ;
#356 = AXIS2_PLACEMENT_3D ( 'NONE', #9538, #13647, #7988 ) ;
#357 = FACE_OUTER_BOUND ( 'NONE', #24183, .T. ) ;
#358 = CARTESIAN_POINT ( 'NONE',  ( 38.37017380507020192, -22.01368208888610312, 72.51602215082118619 ) ) ;
#359 = VECTOR ( 'NONE', #22680, 1000.000000000000000 ) ;
#360 = EDGE_LOOP ( 'NONE', ( #9313, #7335, #23676, #19391, #21590, #5300, #7158, #3362 ) ) ;
#361 = CARTESIAN_POINT ( 'NONE',  ( 39.82744760895728575, -21.57196225014778790, 75.82680905536302873 ) ) ;
#362 = DIRECTION ( 'NONE',  ( -2.385244779468109755E-15, 1.000000000000000000, 0.000000000000000000 ) ) ;
#363 = EDGE_LOOP ( 'NONE', ( #20532, #24029, #12910, #14891, #19447, #20167, #13360, #10230, #14079, #1336, #8917 ) ) ;
#364 = ORIENTED_EDGE ( 'NONE', *, *, #2300, .T. ) ;
#365 = CARTESIAN_POINT ( 'NONE',  ( 40.52078840805429394, -21.00384086642191761, 72.15350918040381600 ) ) ;
#366 = VECTOR ( 'NONE', #18918, 1000.000000000000114 ) ;
#367 = CARTESIAN_POINT ( 'NONE',  ( 39.29254315202756231, -28.81368208888610383, 69.94417936956671156 ) ) ;
#368 = FACE_OUTER_BOUND ( 'NONE', #16968, .T. ) ;
#369 = AXIS2_PLACEMENT_3D ( 'NONE', #5770, #5638, #19552 ) ;
#370 = AXIS2_PLACEMENT_3D ( 'NONE', #22891, #22513, #18525 ) ;
#371 = LINE ( 'NONE', #16872, #11443 ) ;
#372 = ORIENTED_EDGE ( 'NONE', *, *, #24453, .T. ) ;
#373 = DIRECTION ( 'NONE',  ( -1.000000000000000000, -0.000000000000000000, -0.000000000000000000 ) ) ;
#374 = CYLINDRICAL_SURFACE ( 'NONE', #2185, 1.500000000000006217 ) ;
#375 = ADVANCED_FACE ( 'NONE', ( #8387 ), #5942, .F. ) ;
#376 = CARTESIAN_POINT ( 'NONE',  ( 35.86008812008917346, -4.103840866421913702, 71.32335560751961623 ) ) ;
#377 = DIRECTION ( 'NONE',  ( 0.000000000000000000, 0.8212051873014208914, 0.5706330172266919076 ) ) ;
#378 = AXIS2_PLACEMENT_3D ( 'NONE', #5265, #13131, #6123 ) ;
#379 = DIRECTION ( 'NONE',  ( 1.000000000000000000, 0.000000000000000000, 0.000000000000000000 ) ) ;
#380 = CARTESIAN_POINT ( 'NONE',  ( 37.33957961208646736, -7.813682088886109156, 72.81632618279323310 ) ) ;
#381 = LINE ( 'NONE', #10079, #6023 ) ;
#382 = CARTESIAN_POINT ( 'NONE',  ( 33.31606138205700773, -16.48551471403133206, 77.11349248448009064 ) ) ;
#383 = AXIS2_PLACEMENT_3D ( 'NONE', #20572, #5122, #2903 ) ;
#384 = CARTESIAN_POINT ( 'NONE',  ( 40.31606138205700773, 41.44123852234599781, 74.30501292736987295 ) ) ;
#385 = CARTESIAN_POINT ( 'NONE',  ( 36.81606138205700063, 8.691238522346987239, 65.30501292736998664 ) ) ;
#386 = CARTESIAN_POINT ( 'NONE',  ( 38.31606138205694378, 4.312150376739274371, 4.986822452676363149 ) ) ;
#387 = VECTOR ( 'NONE', #11999, 1000.000000000000000 ) ;
#388 = ADVANCED_FACE ( 'NONE', ( #12254 ), #16230, .F. ) ;
#389 = CARTESIAN_POINT ( 'NONE',  ( 39.02742774030101458, -23.40384086642191264, 70.49320253461759478 ) ) ;
#390 = CARTESIAN_POINT ( 'NONE',  ( 39.82603832034400426, -10.31368208888610383, 72.40698646996135324 ) ) ;
#391 = EDGE_CURVE ( 'NONE', #8203, #1835, #13926, .T. ) ;
#392 = CARTESIAN_POINT ( 'NONE',  ( 44.81606138205700063, -38.55876147765400930, 73.30501292737012875 ) ) ;
#393 = CARTESIAN_POINT ( 'NONE',  ( 38.93415946300896024, -9.503840866421908729, 69.66206559358663242 ) ) ;
#394 = ADVANCED_FACE ( 'NONE', ( #12384 ), #4140, .F. ) ;
#395 = CARTESIAN_POINT ( 'NONE',  ( 30.81606138205700418, -26.74044063519535186, 82.50501292737007475 ) ) ;
#396 = APPLICATION_CONTEXT ( 'automotive_design' ) ;
#397 = CARTESIAN_POINT ( 'NONE',  ( 38.26194895904383486, -9.013682088886101340, 69.64448340153879258 ) ) ;
#398 = ORIENTED_EDGE ( 'NONE', *, *, #4868, .T. ) ;
#399 = CARTESIAN_POINT ( 'NONE',  ( 36.11133435605973574, -13.61368208888610454, 72.15350918040385864 ) ) ;
#400 = ORIENTED_EDGE ( 'NONE', *, *, #21408, .T. ) ;
#401 = CARTESIAN_POINT ( 'NONE',  ( 38.44255644662678861, -39.60718113818700203, 83.30501292737011454 ) ) ;
#402 = CARTESIAN_POINT ( 'NONE',  ( 38.31606138205700063, 40.69123852234599781, 71.30501292737000085 ) ) ;
#403 = CARTESIAN_POINT ( 'NONE',  ( 37.12184278917507640, -16.10384086642191193, 71.32335560751961623 ) ) ;
#404 = EDGE_LOOP ( 'NONE', ( #18442, #12105, #307, #7710 ) ) ;
#405 = VECTOR ( 'NONE', #24075, 1000.000000000000000 ) ;
#406 = ORIENTED_EDGE ( 'NONE', *, *, #18732, .F. ) ;
#407 = DIRECTION ( 'NONE',  ( 1.734723475976805122E-16, 3.491481338843134933E-15, 1.000000000000000000 ) ) ;
#408 = DIRECTION ( 'NONE',  ( 0.000000000000000000, 1.000000000000000000, -4.625929269271481378E-15 ) ) ;
#409 = EDGE_CURVE ( 'NONE', #17565, #5522, #244, .T. ) ;
#410 = CARTESIAN_POINT ( 'NONE',  ( 36.89935272106205133, -24.40384086642191974, 73.23812341099225875 ) ) ;
#411 = VECTOR ( 'NONE', #3457, 1000.000000000000227 ) ;
#412 = LINE ( 'NONE', #17964, #14177 ) ;
#413 = CARTESIAN_POINT ( 'NONE',  ( 39.75915168707250302, -26.71368208888609530, 70.26145752964249880 ) ) ;
#414 = FACE_OUTER_BOUND ( 'NONE', #16051, .T. ) ;
#415 = ORIENTED_EDGE ( 'NONE', *, *, #6576, .T. ) ;
#416 = DIRECTION ( 'NONE',  ( -1.000000000000000000, 0.000000000000000000, 0.000000000000000000 ) ) ;
#417 = CARTESIAN_POINT ( 'NONE',  ( 30.81606138205696155, 1.773964314019527588, -3.427682652428149623 ) ) ;
#418 = CARTESIAN_POINT ( 'NONE',  ( 38.93415946300897446, -23.50384086642190340, 69.66206559358663242 ) ) ;
#419 = CYLINDRICAL_SURFACE ( 'NONE', #8765, 0.5000000000000004441 ) ;
#420 = ADVANCED_FACE ( 'NONE', ( #130 ), #10070, .F. ) ;
#421 = ORIENTED_EDGE ( 'NONE', *, *, #16949, .T. ) ;
#422 = EDGE_CURVE ( 'NONE', #6624, #2302, #15968, .T. ) ;
#423 = VECTOR ( 'NONE', #2307, 1000.000000000000000 ) ;
#424 = PLANE ( 'NONE',  #3641 ) ;
#425 = ADVANCED_FACE ( 'NONE', ( #18305 ), #23824, .T. ) ;
#426 = AXIS2_PLACEMENT_3D ( 'NONE', #23503, #3937, #7679 ) ;
#427 = DIRECTION ( 'NONE',  ( 2.690219486203388234E-15, -0.8967398287344627850, -0.4425581086832399147 ) ) ;
#428 = ADVANCED_FACE ( 'NONE', ( #6197 ), #2308, .T. ) ;
#429 = CARTESIAN_POINT ( 'NONE',  ( 39.75915168707251723, -28.90384086642191619, 72.49904802271737481 ) ) ;
#430 = ADVANCED_FACE ( 'NONE', ( #17799 ), #14051, .T. ) ;
#431 = CARTESIAN_POINT ( 'NONE',  ( 36.31606138205700063, -30.30876147765400574, 73.55501292737010033 ) ) ;
#432 = EDGE_LOOP ( 'NONE', ( #18216, #5933, #5741, #16372 ) ) ;
#433 = CYLINDRICAL_SURFACE ( 'NONE', #4572, 0.7500000000000093259 ) ;
#434 = ORIENTED_EDGE ( 'NONE', *, *, #3015, .T. ) ;
#435 = ORIENTED_EDGE ( 'NONE', *, *, #25058, .T. ) ;
#436 = PLANE ( 'NONE',  #12761 ) ;
#437 = DIRECTION ( 'NONE',  ( 0.000000000000000000, 1.000000000000000000, -6.938893903907222067E-15 ) ) ;
#438 = UNCERTAINTY_MEASURE_WITH_UNIT (LENGTH_MEASURE( 1.000000000000000082E-05 ), #6854, 'distance_accuracy_value', 'NONE');
#439 = CARTESIAN_POINT ( 'NONE',  ( 37.89291511884476904, -5.113682088886100985, 70.26206559358664094 ) ) ;
#440 = CARTESIAN_POINT ( 'NONE',  ( 37.38336156205274818, -1.713682088886100852, 72.12822762946751709 ) ) ;
#441 = ORIENTED_EDGE ( 'NONE', *, *, #10566, .F. ) ;
#442 = ORIENTED_EDGE ( 'NONE', *, *, #7387, .T. ) ;
#443 = LINE ( 'NONE', #18607, #21420 ) ;
#444 = LINE ( 'NONE', #22224, #5450 ) ;
#445 = ORIENTED_EDGE ( 'NONE', *, *, #19266, .F. ) ;
#446 = EDGE_CURVE ( 'NONE', #545, #18597, #371, .T. ) ;
#447 = CARTESIAN_POINT ( 'NONE',  ( 3.816061382056971762, -5.229446354161006560, -9.573232046949398111 ) ) ;
#448 = CARTESIAN_POINT ( 'NONE',  ( 39.38009889167648936, -11.40384086642190908, 70.00779233799264034 ) ) ;
#449 = CARTESIAN_POINT ( 'NONE',  ( 35.31606138205687273, 42.19123852234595518, 61.80501292736988006 ) ) ;
#450 = CARTESIAN_POINT ( 'NONE',  ( 36.31606138205700063, -20.32227907754186802, 76.00185088427946312 ) ) ;
#451 = CARTESIAN_POINT ( 'NONE',  ( 33.80827534892208064, -18.91453975041207158, 24.37026150481227305 ) ) ;
#452 = EDGE_LOOP ( 'NONE', ( #22783, #2146, #1836, #8004 ) ) ;
#453 = ORIENTED_EDGE ( 'NONE', *, *, #20893, .T. ) ;
#454 = AXIS2_PLACEMENT_3D ( 'NONE', #10382, #13746, #10009 ) ;
#455 = ORIENTED_EDGE ( 'NONE', *, *, #16653, .F. ) ;
#456 = CARTESIAN_POINT ( 'NONE',  ( 36.31606138205700063, 43.19123852234599781, 74.30501292736987295 ) ) ;
#457 = CARTESIAN_POINT ( 'NONE',  ( 40.14115730948191185, -6.513682088886103116, 71.32335560751961623 ) ) ;
#458 = EDGE_CURVE ( 'NONE', #22083, #20938, #22536, .T. ) ;
#459 = CARTESIAN_POINT ( 'NONE',  ( 33.66606138205698073, -6.570990706613086374, -2.335727660491067503 ) ) ;
#460 = CARTESIAN_POINT ( 'NONE',  ( 36.81465384343994884, 41.67000142393845152, 79.87823623207322044 ) ) ;
#461 = DIRECTION ( 'NONE',  ( -0.000000000000000000, 0.1904761904761826663, -0.9816918156232541381 ) ) ;
#462 = DIRECTION ( 'NONE',  ( 1.000000000000000000, 3.614007241618344826E-17, -1.084202172485503317E-31 ) ) ;
#463 = PRODUCT_DEFINITION_SHAPE ( 'NONE', 'NONE',  #25490 ) ;
#464 = DIRECTION ( 'NONE',  ( -1.734723475976814737E-16, -3.009265538105065873E-32, -1.000000000000000000 ) ) ;
#465 = DIRECTION ( 'NONE',  ( 0.000000000000000000, -0.1918498038142812112, 0.9814242980364923374 ) ) ;
#466 = CARTESIAN_POINT ( 'NONE',  ( 33.56606138205700773, 43.19123852234599781, 75.30501292736987295 ) ) ;
#467 = VERTEX_POINT ( 'NONE', #6689 ) ;
#468 = EDGE_LOOP ( 'NONE', ( #17209, #1468 ) ) ;
#469 = DIRECTION ( 'NONE',  ( 1.444147469618246167E-16, -0.8212051873014210024, -0.5706330172266920187 ) ) ;
#470 = CARTESIAN_POINT ( 'NONE',  ( 39.73277004305197124, -3.403840866421911748, 69.52238214136768590 ) ) ;
#471 = ORIENTED_EDGE ( 'NONE', *, *, #5498, .T. ) ;
#472 = AXIS2_PLACEMENT_3D ( 'NONE', #1050, #9195, #18717 ) ;
#473 = CARTESIAN_POINT ( 'NONE',  ( 31.81606138205700418, -22.55876147765401996, 68.80501292737008612 ) ) ;
#474 = CARTESIAN_POINT ( 'NONE',  ( 37.25202387243752611, -7.213682088886102406, 70.00779233799264034 ) ) ;
#475 = DIRECTION ( 'NONE',  ( 0.000000000000000000, 1.000000000000000000, -2.775557561562891351E-15 ) ) ;
#476 = CARTESIAN_POINT ( 'NONE',  ( 39.64521430340304420, -14.81368208888610205, 69.45876917294175712 ) ) ;
#477 = EDGE_CURVE ( 'NONE', #16296, #2532, #6909, .T. ) ;
#478 = FACE_OUTER_BOUND ( 'NONE', #5733, .T. ) ;
#479 = EDGE_CURVE ( 'NONE', #15938, #12825, #16471, .T. ) ;
#480 = DIRECTION ( 'NONE',  ( 1.327674326049719602E-15, -0.4425581086832399147, 0.8967398287344627850 ) ) ;
#481 = AXIS2_PLACEMENT_3D ( 'NONE', #1514, #19059, #7211 ) ;
#482 = CARTESIAN_POINT ( 'NONE',  ( 40.31606138205701484, -21.38339321089542011, 27.67811916372966863 ) ) ;
#483 =( NAMED_UNIT ( * ) PLANE_ANGLE_UNIT ( ) SI_UNIT ( $, .RADIAN. ) );
#484 = DIRECTION ( 'NONE',  ( -1.000000000000000000, 0.000000000000000000, 0.000000000000000000 ) ) ;
#485 = TOROIDAL_SURFACE ( 'NONE', #1324, 1.000000000000000000, 1.000000000000000000 ) ;
#486 = PLANE ( 'NONE',  #5925 ) ;
#487 = DIRECTION ( 'NONE',  ( -1.000000000000000000, 0.000000000000000000, 0.000000000000000000 ) ) ;
#488 = CARTESIAN_POINT ( 'NONE',  ( 39.41296390513587511, -24.41368208888610525, 71.67976084211548482 ) ) ;
#489 = ORIENTED_EDGE ( 'NONE', *, *, #13595, .T. ) ;
#490 = CARTESIAN_POINT ( 'NONE',  ( 38.83707137437546919, -22.15663359646540087, 75.30013868356464002 ) ) ;
#491 = EDGE_CURVE ( 'NONE', #22735, #4487, #20477, .T. ) ;
#492 = LINE ( 'NONE', #619, #7832 ) ;
#493 = ORIENTED_EDGE ( 'NONE', *, *, #7515, .F. ) ;
#494 = ORIENTED_EDGE ( 'NONE', *, *, #8342, .T. ) ;
#495 = CARTESIAN_POINT ( 'NONE',  ( 36.89935272106205133, -22.40384086642191974, 73.23812341099225875 ) ) ;
#496 = CARTESIAN_POINT ( 'NONE',  ( 38.26194895904383486, -27.01368208888610312, 69.64448340153876416 ) ) ;
#497 = PLANE ( 'NONE',  #7863 ) ;
#498 = VECTOR ( 'NONE', #21104, 1000.000000000000114 ) ;
#499 = LINE ( 'NONE', #627, #16776 ) ;
#500 = DIRECTION ( 'NONE',  ( 1.000000000000000000, 0.000000000000000000, 0.000000000000000000 ) ) ;
#501 = ORIENTED_EDGE ( 'NONE', *, *, #9098, .T. ) ;
#502 = LINE ( 'NONE', #5275, #212 ) ;
#503 = DIRECTION ( 'NONE',  ( 0.000000000000000000, -3.491481338843135327E-15, -1.000000000000000000 ) ) ;
#504 = VECTOR ( 'NONE', #8993, 1000.000000000000000 ) ;
#505 = CARTESIAN_POINT ( 'NONE',  ( 38.26194895904384197, -2.603840866421920364, 73.71602215082116061 ) ) ;
#506 = ADVANCED_FACE ( 'NONE', ( #12517 ), #18548, .T. ) ;
#507 = DIRECTION ( 'NONE',  ( -0.000000000000000000, 1.000000000000000000, 0.000000000000000000 ) ) ;
#509 = EDGE_CURVE ( 'NONE', #23982, #20593, #22128, .T. ) ;
#508 = DIRECTION ( 'NONE',  ( 0.000000000000000000, -3.269436733918100469E-15, -1.000000000000000000 ) ) ;
#510 = CARTESIAN_POINT ( 'NONE',  ( 39.38009889167650357, -8.213682088886105959, 72.75271321436733274 ) ) ;
#511 = DIRECTION ( 'NONE',  ( 1.734723475976804876E-16, 3.491481338843135327E-15, 1.000000000000000000 ) ) ;
#512 = VECTOR ( 'NONE', #1905, 1000.000000000000227 ) ;
#513 = AXIS2_PLACEMENT_3D ( 'NONE', #8102, #24168, #14160 ) ;
#514 = CARTESIAN_POINT ( 'NONE',  ( 33.31606138205700773, -20.26871824316192061, 44.92082169825412308 ) ) ;
#515 = CARTESIAN_POINT ( 'NONE',  ( 32.81606138205700773, 35.38401127291550097, 61.48364296169660292 ) ) ;
#516 = AXIS2_PLACEMENT_3D ( 'NONE', #2871, #20924, #11140 ) ;
#517 = CONTEXT_DEPENDENT_SHAPE_REPRESENTATION ( #23280, #12214 ) ;
#518 = AXIS2_PLACEMENT_3D ( 'NONE', #8054, #21699, #12437 ) ;
#519 = CARTESIAN_POINT ( 'NONE',  ( 31.01606138205699992, 44.92314894770294131, 81.17823623207320338 ) ) ;
#520 = CARTESIAN_POINT ( 'NONE',  ( 39.41296390513587511, -23.20384086642191335, 71.08074471024441721 ) ) ;
#521 = CARTESIAN_POINT ( 'NONE',  ( 36.64852494920107517, -13.41368208888610525, 70.89533451361947414 ) ) ;
#522 = DIRECTION ( 'NONE',  ( -1.000000000000000000, 0.000000000000000000, 0.000000000000000000 ) ) ;
#523 = EDGE_CURVE ( 'NONE', #15010, #2216, #1011, .T. ) ;
#524 = CARTESIAN_POINT ( 'NONE',  ( 36.68196826583682935, -14.00384086642191228, 70.79240656858107172 ) ) ;
#525 = DIRECTION ( 'NONE',  ( 0.000000000000000000, 1.000000000000000000, -2.999999999999999839E-15 ) ) ;
#526 = AXIS2_PLACEMENT_3D ( 'NONE', #704, #5104, #14630 ) ;
#527 = CARTESIAN_POINT ( 'NONE',  ( 37.25202387243752611, -11.21368208888610241, 70.00779233799262613 ) ) ;
#528 = ORIENTED_EDGE ( 'NONE', *, *, #18616, .T. ) ;
#529 = CARTESIAN_POINT ( 'NONE',  ( 40.26954217208371034, -18.71368208888610241, 69.89063713639258424 ) ) ;
#530 = EDGE_LOOP ( 'NONE', ( #17922, #3533, #2092, #3855 ) ) ;
#531 = FACE_OUTER_BOUND ( 'NONE', #15557, .T. ) ;
#532 = FACE_BOUND ( 'NONE', #6040, .T. ) ;
#533 = CARTESIAN_POINT ( 'NONE',  ( 38.26194895904384197, -16.60384086642191193, 72.51602215082118619 ) ) ;
#534 = STYLED_ITEM ( 'NONE', ( #16830 ), #19676 ) ;
#535 = ORIENTED_EDGE ( 'NONE', *, *, #15892, .T. ) ;
#536 = VERTEX_POINT ( 'NONE', #10946 ) ;
#537 = FACE_OUTER_BOUND ( 'NONE', #20506, .T. ) ;
#538 = PLANE ( 'NONE',  #4659 ) ;
#539 = CARTESIAN_POINT ( 'NONE',  ( 36.11133435605973574, -26.00384086642192116, 70.60699637195608602 ) ) ;
#540 = CIRCLE ( 'NONE', #15353, 0.9999999999999940048 ) ;
#541 = CARTESIAN_POINT ( 'NONE',  ( 31.81606138205700418, 38.19123852234599070, 72.05501292736988717 ) ) ;
#542 = CARTESIAN_POINT ( 'NONE',  ( 38.82593461698262871, -24.91368208888610170, 69.62690120949091011 ) ) ;
#543 = AXIS2_PLACEMENT_3D ( 'NONE', #16608, #5020, #14671 ) ;
#544 = FACE_OUTER_BOUND ( 'NONE', #14731, .T. ) ;
#545 = VERTEX_POINT ( 'NONE', #10703 ) ;
#546 = VERTEX_POINT ( 'NONE', #873 ) ;
#547 = DIRECTION ( 'NONE',  ( 0.000000000000000000, -3.491481338843135327E-15, -1.000000000000000000 ) ) ;
#548 = DIRECTION ( 'NONE',  ( -8.381647117973248681E-31, -0.7071067811865460184, -0.7071067811865489050 ) ) ;
#549 = VECTOR ( 'NONE', #9794, 1000.000000000000000 ) ;
#550 = CARTESIAN_POINT ( 'NONE',  ( 36.87297107704151244, -11.90384086642190908, 70.26145752964255564 ) ) ;
#551 = DIRECTION ( 'NONE',  ( 1.000000000000000000, 0.000000000000000000, 0.000000000000000000 ) ) ;
#552 =( GEOMETRIC_REPRESENTATION_CONTEXT ( 3 ) GLOBAL_UNCERTAINTY_ASSIGNED_CONTEXT ( ( #3328 ) ) GLOBAL_UNIT_ASSIGNED_CONTEXT ( ( #4972, #12369, #1089 ) ) REPRESENTATION_CONTEXT ( 'NONE', 'WORKASPACE' ) );
#553 = DIRECTION ( 'NONE',  ( 0.000000000000000000, 2.999999999999999839E-15, 1.000000000000000000 ) ) ;
#554 = EDGE_CURVE ( 'NONE', #25393, #22104, #18436, .T. ) ;
#555 = AXIS2_PLACEMENT_3D ( 'NONE', #19698, #6310, #13908 ) ;
#556 = DIRECTION ( 'NONE',  ( 0.000000000000000000, -0.8212051873014223347, -0.5706330172266899092 ) ) ;
#557 = CARTESIAN_POINT ( 'NONE',  ( 38.63098279924290068, -0.7038408664219106825, 72.53360434286905445 ) ) ;
#558 = CARTESIAN_POINT ( 'NONE',  ( 38.31606138205700063, 37.69123852234599781, 71.30501292737001506 ) ) ;
#559 = VERTEX_POINT ( 'NONE', #14427 ) ;
#560 = AXIS2_PLACEMENT_3D ( 'NONE', #2943, #9027, #8898 ) ;
#561 = LINE ( 'NONE', #184, #3329 ) ;
#562 = VERTEX_POINT ( 'NONE', #2686 ) ;
#563 = ORIENTED_EDGE ( 'NONE', *, *, #20158, .T. ) ;
#564 = CARTESIAN_POINT ( 'NONE',  ( 36.06606138205700063, 3.151453266960317023, 6.397347472316774031 ) ) ;
#565 = DIRECTION ( 'NONE',  ( 0.000000000000000000, 0.000000000000000000, 1.000000000000000000 ) ) ;
#566 = CARTESIAN_POINT ( 'NONE',  ( 37.60469502381300089, -7.213682088886102406, 70.49320253461759478 ) ) ;
#567 = CARTESIAN_POINT ( 'NONE',  ( 39.24876120206128860, -4.713682088886099741, 70.63227792289247020 ) ) ;
#568 = ORIENTED_EDGE ( 'NONE', *, *, #2920, .F. ) ;
#569 = ORIENTED_EDGE ( 'NONE', *, *, #16312, .T. ) ;
#570 = DIRECTION ( 'NONE',  ( 0.000000000000000000, 1.000000000000000000, -2.999999999999999839E-15 ) ) ;
#571 = CYLINDRICAL_SURFACE ( 'NONE', #12870, 1.749999999999998668 ) ;
#572 = CARTESIAN_POINT ( 'NONE',  ( 32.31606138205700063, -20.55619265724211076, 44.11584019928223910 ) ) ;
#573 = CARTESIAN_POINT ( 'NONE',  ( 37.25202387243754032, -12.40384086642191619, 72.75271321436731853 ) ) ;
#574 = EDGE_CURVE ( 'NONE', #16761, #23326, #24565, .T. ) ;
#575 = DIRECTION ( 'NONE',  ( 1.000000000000000000, 2.440719103442460911E-15, 1.328886038262200866E-15 ) ) ;
#576 = PRESENTATION_LAYER_ASSIGNMENT (  '', '', ( #9255 ) ) ;
#577 = ADVANCED_FACE ( 'NONE', ( #16345 ), #8767, .F. ) ;
#578 = CARTESIAN_POINT ( 'NONE',  ( 38.31606138205700063, 37.69123852234599781, 71.30501292737001506 ) ) ;
#579 = ADVANCED_FACE ( 'NONE', ( #24194 ), #4638, .F. ) ;
#580 = ORIENTED_EDGE ( 'NONE', *, *, #7197, .F. ) ;
#581 = CIRCLE ( 'NONE', #14988, 1.500000000000001332 ) ;
#582 = EDGE_LOOP ( 'NONE', ( #9120, #20144, #14940, #6594 ) ) ;
#583 = EDGE_CURVE ( 'NONE', #22400, #7712, #22663, .T. ) ;
#584 = EDGE_CURVE ( 'NONE', #10773, #7324, #23762, .T. ) ;
#585 = ORIENTED_EDGE ( 'NONE', *, *, #15854, .T. ) ;
#586 = DIRECTION ( 'NONE',  ( 0.000000000000000000, -0.7540134720837717852, -0.6568589528324746407 ) ) ;
#587 = CARTESIAN_POINT ( 'NONE',  ( 37.25202387243752611, -7.213682088886102406, 70.00779233799264034 ) ) ;
#588 = CIRCLE ( 'NONE', #8830, 10.00000000000000000 ) ;
#589 = CARTESIAN_POINT ( 'NONE',  ( 39.93978280207628018, -29.10876147765328525, 71.30174507665321926 ) ) ;
#590 = CARTESIAN_POINT ( 'NONE',  ( 33.40064408022072939, 42.38065457974295924, 79.52109337493035923 ) ) ;
#591 = CARTESIAN_POINT ( 'NONE',  ( 37.25202387243752611, -27.21368208888610241, 70.00779233799262613 ) ) ;
#592 = DIRECTION ( 'NONE',  ( 0.000000000000000000, -0.5706330172266919076, 0.8212051873014208914 ) ) ;
#593 = EDGE_CURVE ( 'NONE', #5442, #4334, #1137, .T. ) ;
#594 = EDGE_CURVE ( 'NONE', #6472, #12687, #11972, .T. ) ;
#595 = DIRECTION ( 'NONE',  ( -1.836970198721029688E-16, -2.999999999999999839E-15, -1.000000000000000000 ) ) ;
#596 = DIRECTION ( 'NONE',  ( 1.000000000000000000, -5.204170427930415223E-30, -1.734723475976805122E-15 ) ) ;
#597 = CARTESIAN_POINT ( 'NONE',  ( 36.57685537766501227, -21.21804332987624875, 75.35486877457063315 ) ) ;
#598 = ORIENTED_EDGE ( 'NONE', *, *, #10845, .F. ) ;
#599 = ORIENTED_EDGE ( 'NONE', *, *, #18942, .T. ) ;
#600 = AXIS2_PLACEMENT_3D ( 'NONE', #19096, #2975, #3368 ) ;
#601 = CARTESIAN_POINT ( 'NONE',  ( 32.81606138205700773, 6.705285648480822758, 7.416521610403067122 ) ) ;
#602 = CARTESIAN_POINT ( 'NONE',  ( 36.98690846071097127, -1.803840866421911215, 69.45876917294177133 ) ) ;
#603 = CARTESIAN_POINT ( 'NONE',  ( 38.37017380507020192, -26.01368208888610312, 72.51602215082114355 ) ) ;
#604 = ORIENTED_EDGE ( 'NONE', *, *, #15336, .F. ) ;
#605 = EDGE_LOOP ( 'NONE', ( #8949, #22189, #20198, #2594 ) ) ;
#606 = CARTESIAN_POINT ( 'NONE',  ( 41.31606138205700063, 7.864187680719676443, 65.89022736311019912 ) ) ;
#607 = CARTESIAN_POINT ( 'NONE',  ( 37.25202387243752611, -9.213682088886100630, 70.00779233799264034 ) ) ;
#608 = CARTESIAN_POINT ( 'NONE',  ( 38.26194895904384907, -28.60384086642191548, 73.11602215082115208 ) ) ;
#609 = FACE_OUTER_BOUND ( 'NONE', #22404, .T. ) ;
#610 = CARTESIAN_POINT ( 'NONE',  ( 40.33642880535524000, -10.31368208888610738, 72.77780686321128201 ) ) ;
#611 = LINE ( 'NONE', #20075, #6527 ) ;
#612 = CARTESIAN_POINT ( 'NONE',  ( 46.81606138205702905, -23.83075694525939170, 32.63712566015296090 ) ) ;
#613 = CIRCLE ( 'NONE', #19551, 0.2314957320545540931 ) ;
#614 = DIRECTION ( 'NONE',  ( 0.000000000000000000, 1.000000000000000000, -3.491481338843134933E-15 ) ) ;
#615 = LINE ( 'NONE', #21762, #11077 ) ;
#616 = LINE ( 'NONE', #20345, #10667 ) ;
#617 = ORIENTED_EDGE ( 'NONE', *, *, #1775, .T. ) ;
#618 = CARTESIAN_POINT ( 'NONE',  ( 40.31606138205700773, -20.48183877227857508, 75.44871329660013259 ) ) ;
#619 = CARTESIAN_POINT ( 'NONE',  ( 43.23147868389327897, 40.76768529863396395, 79.37823623207322044 ) ) ;
#620 = ORIENTED_EDGE ( 'NONE', *, *, #4318, .T. ) ;
#621 = ORIENTED_EDGE ( 'NONE', *, *, #6367, .T. ) ;
#622 = CARTESIAN_POINT ( 'NONE',  ( 36.29569395875881099, -22.30384086642192187, 72.77780686321128201 ) ) ;
#623 = EDGE_CURVE ( 'NONE', #5929, #22719, #8597, .T. ) ;
#624 = CARTESIAN_POINT ( 'NONE',  ( 38.82593461698262871, -28.91368208888610525, 69.62690120949091011 ) ) ;
#625 = EDGE_CURVE ( 'NONE', #9404, #8440, #1536, .T. ) ;
#626 = LINE ( 'NONE', #2187, #423 ) ;
#627 = CARTESIAN_POINT ( 'NONE',  ( 29.71606138205698500, -6.548589660139427338, -8.069948661059612505 ) ) ;
#628 = LINE ( 'NONE', #17704, #1167 ) ;
#629 = EDGE_LOOP ( 'NONE', ( #17511, #10756, #22625, #6939, #1629, #11779, #9994, #21905 ) ) ;
#630 = CARTESIAN_POINT ( 'NONE',  ( 32.81606138205700773, -35.82531359714782582, 71.25150419970752580 ) ) ;
#631 = CARTESIAN_POINT ( 'NONE',  ( 28.81606138205695444, -23.19619402982950263, 47.16846523730000484 ) ) ;
#632 = CARTESIAN_POINT ( 'NONE',  ( 39.73277004305197124, -3.403840866421911748, 69.52238214136768590 ) ) ;
#633 = DIRECTION ( 'NONE',  ( 1.445602896647339656E-16, -0.8212051873014208914, -0.5706330172266919076 ) ) ;
#634 = LINE ( 'NONE', #22037, #2547 ) ;
#635 = CARTESIAN_POINT ( 'NONE',  ( 40.14115730948191185, -10.51368208888609956, 71.32335560751961623 ) ) ;
#636 = DIRECTION ( 'NONE',  ( -7.966588320977881105E-33, 1.000000000000000000, -6.123233995736769734E-17 ) ) ;
#637 = CARTESIAN_POINT ( 'NONE',  ( 37.25202387243752611, -19.21368208888610241, 70.00779233799262613 ) ) ;
#638 = LINE ( 'NONE', #8521, #20462 ) ;
#639 = LINE ( 'NONE', #22551, #16599 ) ;
#640 = CARTESIAN_POINT ( 'NONE',  ( 37.25260217561390874, -24.00384086642191761, 70.97781676520601479 ) ) ;
#641 = CARTESIAN_POINT ( 'NONE',  ( 39.75915168707250302, -10.71368208888609885, 70.26145752964252722 ) ) ;
#642 = AXIS2_PLACEMENT_3D ( 'NONE', #14194, #22039, #12393 ) ;
#643 = VERTEX_POINT ( 'NONE', #12347 ) ;
#644 = CARTESIAN_POINT ( 'NONE',  ( 33.57054761034910229, 3.412271088041349820, 6.349711998884802533 ) ) ;
#645 = ORIENTED_EDGE ( 'NONE', *, *, #2860, .F. ) ;
#646 = ADVANCED_FACE ( 'NONE', ( #14389 ), #335, .T. ) ;
#647 = CARTESIAN_POINT ( 'NONE',  ( 39.98359781491296161, -9.203840866421911571, 70.89533451361947414 ) ) ;
#648 = PLANE ( 'NONE',  #1506 ) ;
#649 = EDGE_CURVE ( 'NONE', #18044, #10390, #12216, .T. ) ;
#650 = EDGE_CURVE ( 'NONE', #5870, #848, #10535, .T. ) ;
#651 = CARTESIAN_POINT ( 'NONE',  ( 36.68196826583682935, -3.613682088886103205, 71.96809898377890136 ) ) ;
#652 = EDGE_LOOP ( 'NONE', ( #17580, #11877, #24697, #22252 ) ) ;
#653 = CARTESIAN_POINT ( 'NONE',  ( 40.55423172469004811, -16.41368208888610525, 72.05058123536544201 ) ) ;
#654 = ORIENTED_EDGE ( 'NONE', *, *, #13211, .F. ) ;
#655 = DIRECTION ( 'NONE',  ( -1.000000000000000000, -3.043523379167283935E-15, -1.423844882595663967E-16 ) ) ;
#656 = LINE ( 'NONE', #2341, #117 ) ;
#657 = CARTESIAN_POINT ( 'NONE',  ( 38.63098279924290068, -18.70384086642191335, 72.53360434286904024 ) ) ;
#658 = EDGE_LOOP ( 'NONE', ( #5985, #10413, #8337, #20417 ) ) ;
#659 = ORIENTED_EDGE ( 'NONE', *, *, #11638, .T. ) ;
#660 = DIRECTION ( 'NONE',  ( -1.000000000000000000, 0.000000000000000000, 1.734723475976804876E-16 ) ) ;
#661 = DIRECTION ( 'NONE',  ( -1.000000000000000000, 0.000000000000000000, 1.734723475976804876E-16 ) ) ;
#662 = CARTESIAN_POINT ( 'NONE',  ( 39.73277004305197124, -21.40384086642191619, 69.52238214136768590 ) ) ;
#663 = DIRECTION ( 'NONE',  ( 1.000000000000000000, 0.000000000000000000, 0.000000000000000000 ) ) ;
#664 = CARTESIAN_POINT ( 'NONE',  ( 38.37017380507020192, -26.01368208888611022, 73.11602215082115208 ) ) ;
#665 = LINE ( 'NONE', #21852, #15394 ) ;
#666 = EDGE_CURVE ( 'NONE', #2759, #3821, #18380, .T. ) ;
#667 = FACE_OUTER_BOUND ( 'NONE', #25437, .T. ) ;
#668 = ORIENTED_EDGE ( 'NONE', *, *, #7604, .F. ) ;
#669 = FACE_OUTER_BOUND ( 'NONE', #20627, .T. ) ;
#670 = CYLINDRICAL_SURFACE ( 'NONE', #10166, 9.500000000000000000 ) ;
#671 = CARTESIAN_POINT ( 'NONE',  ( 37.25202387243754032, -16.40384086642191619, 72.75271321436731853 ) ) ;
#672 = DIRECTION ( 'NONE',  ( 0.000000000000000000, 0.000000000000000000, 1.000000000000000000 ) ) ;
#673 = CARTESIAN_POINT ( 'NONE',  ( 34.56606138205700773, 41.44123852234599781, 74.30501292736987295 ) ) ;
#674 = VECTOR ( 'NONE', #14592, 1000.000000000000000 ) ;
#675 = CARTESIAN_POINT ( 'NONE',  ( 36.31606138205700063, 37.44123852234599781, 74.30501292736988717 ) ) ;
#676 = DIRECTION ( 'NONE',  ( 1.000000000000000000, 0.000000000000000000, 0.000000000000000000 ) ) ;
#677 = CARTESIAN_POINT ( 'NONE',  ( 39.95015449827720744, -29.00384086642191406, 71.96809898377885872 ) ) ;
#678 = CARTESIAN_POINT ( 'NONE',  ( 38.31606138205700063, -22.22127907754186893, 75.80501292736997243 ) ) ;
#679 = ORIENTED_EDGE ( 'NONE', *, *, #2955, .F. ) ;
#680 = CARTESIAN_POINT ( 'NONE',  ( 38.93415946300897446, -24.11368208888610454, 73.09843995877328382 ) ) ;
#681 = ORIENTED_EDGE ( 'NONE', *, *, #198, .T. ) ;
#682 = ORIENTED_EDGE ( 'NONE', *, *, #24180, .T. ) ;
#683 = LINE ( 'NONE', #22085, #3287 ) ;
#684 = LINE ( 'NONE', #8319, #13350 ) ;
#685 = UNCERTAINTY_MEASURE_WITH_UNIT (LENGTH_MEASURE( 1.000000000000000082E-05 ), #25478, 'distance_accuracy_value', 'NONE');
#686 = CARTESIAN_POINT ( 'NONE',  ( 37.25260217561390874, -5.613682088886101873, 71.78268878715394408 ) ) ;
#687 = CARTESIAN_POINT ( 'NONE',  ( 37.38336156205274818, -3.713682088886102406, 72.12822762946751709 ) ) ;
#688 = ORIENTED_EDGE ( 'NONE', *, *, #4557, .F. ) ;
#689 = ORIENTED_EDGE ( 'NONE', *, *, #21380, .T. ) ;
#690 = CARTESIAN_POINT ( 'NONE',  ( 32.81606138205700773, 2.191238522347000117, 69.30501292737000085 ) ) ;
#691 = DIRECTION ( 'NONE',  ( 0.000000000000000000, -0.5706330172266919076, 0.8212051873014208914 ) ) ;
#692 = EDGE_LOOP ( 'NONE', ( #13673, #1108, #11272, #13353 ) ) ;
#693 =( NAMED_UNIT ( * ) PLANE_ANGLE_UNIT ( ) SI_UNIT ( $, .RADIAN. ) );
#694 = CARTESIAN_POINT ( 'NONE',  ( 36.80608444377001831, -12.30384086642191299, 72.40698646996135324 ) ) ;
#695 = VECTOR ( 'NONE', #8729, 1000.000000000000000 ) ;
#696 = AXIS2_PLACEMENT_3D ( 'NONE', #4403, #12150, #17812 ) ;
#697 = VECTOR ( 'NONE', #20975, 999.9999999999998863 ) ;
#698 = DIRECTION ( 'NONE',  ( 0.000000000000000000, -0.6568589528324746407, 0.7540134720837716742 ) ) ;
#699 = EDGE_CURVE ( 'NONE', #20637, #17728, #13096, .T. ) ;
#700 = DIRECTION ( 'NONE',  ( 0.000000000000000000, 0.000000000000000000, -1.000000000000000000 ) ) ;
#701 = ORIENTED_EDGE ( 'NONE', *, *, #6875, .T. ) ;
#702 = ORIENTED_EDGE ( 'NONE', *, *, #17759, .F. ) ;
#703 = ORIENTED_EDGE ( 'NONE', *, *, #3804, .F. ) ;
#704 = CARTESIAN_POINT ( 'NONE',  ( 45.81606138205697221, -4.589472609077215104, -6.350807634294793225 ) ) ;
#705 = CARTESIAN_POINT ( 'NONE',  ( 37.25202387243752611, -5.213682088886100630, 70.00779233799264034 ) ) ;
#706 = FACE_OUTER_BOUND ( 'NONE', #16935, .T. ) ;
#707 = DIRECTION ( 'NONE',  ( -9.027796614315171564E-31, -1.000000000000000000, -3.938893903907230117E-15 ) ) ;
#708 = PLANE ( 'NONE',  #13919 ) ;
#709 = CARTESIAN_POINT ( 'NONE',  ( 29.81606138205697221, -3.984974717493133145, -3.847356352999882656 ) ) ;
#710 = FACE_OUTER_BOUND ( 'NONE', #21187, .T. ) ;
#711 = EDGE_CURVE ( 'NONE', #7305, #21390, #8216, .T. ) ;
#712 = VECTOR ( 'NONE', #15259, 1000.000000000000000 ) ;
#713 = CIRCLE ( 'NONE', #8125, 2.500000000000002220 ) ;
#714 = EDGE_CURVE ( 'NONE', #8686, #3839, #3199, .T. ) ;
#715 = CARTESIAN_POINT ( 'NONE',  ( 37.09022467844553006, -21.80678508585893027, 75.31333329042418256 ) ) ;
#716 = ORIENTED_EDGE ( 'NONE', *, *, #3484, .F. ) ;
#717 = EDGE_CURVE ( 'NONE', #11800, #9537, #10630, .T. ) ;
#718 = EDGE_LOOP ( 'NONE', ( #8864, #2817, #9327, #12481 ) ) ;
#719 = DIRECTION ( 'NONE',  ( 1.000000000000000000, 0.000000000000000000, 0.000000000000000000 ) ) ;
#720 = CARTESIAN_POINT ( 'NONE',  ( 40.52078840805428683, -26.61368208888610809, 70.60699637195608602 ) ) ;
#721 = EDGE_CURVE ( 'NONE', #5120, #2117, #13915, .T. ) ;
#722 = CARTESIAN_POINT ( 'NONE',  ( 38.26194895904383486, -25.01368208888610312, 70.24448340153875847 ) ) ;
#723 = VERTEX_POINT ( 'NONE', #8092 ) ;
#724 = ORIENTED_EDGE ( 'NONE', *, *, #19582, .F. ) ;
#725 = PLANE ( 'NONE',  #8329 ) ;
#726 = CARTESIAN_POINT ( 'NONE',  ( 39.95015449827720744, -4.613682088886104538, 70.79240656858107172 ) ) ;
#727 = CARTESIAN_POINT ( 'NONE',  ( 39.38009889167648936, -27.40384086642190908, 70.00779233799262613 ) ) ;
#728 = DIRECTION ( 'NONE',  ( 0.000000000000000000, -1.000000000000000000, 2.999999999999999839E-15 ) ) ;
#729 = EDGE_CURVE ( 'NONE', #4335, #24890, #4481, .T. ) ;
#730 = CARTESIAN_POINT ( 'NONE',  ( 37.50301148336529167, -7.113682088886103649, 69.06206559358666652 ) ) ;
#731 = VECTOR ( 'NONE', #465, 1000.000000000000227 ) ;
#732 =( BOUNDED_CURVE ( )  B_SPLINE_CURVE ( 3, ( #2177, #11606, #21769, #236 ),
 .UNSPECIFIED., .F., .T. ) 
 B_SPLINE_CURVE_WITH_KNOTS ( ( 4, 4 ),
 ( 0.000000000000000000, 1.570796326794895004 ),
 .UNSPECIFIED. ) 
 CURVE ( )  GEOMETRIC_REPRESENTATION_ITEM ( )  RATIONAL_B_SPLINE_CURVE ( ( 1.000000000000000000, 0.8047378541243649375, 0.8047378541243649375, 1.000000000000000000 ) ) 
 REPRESENTATION_ITEM ( '' )  );
#733 = DIRECTION ( 'NONE',  ( -1.000000000000000000, -2.999999999999999839E-15, 0.000000000000000000 ) ) ;
#734 = CIRCLE ( 'NONE', #8109, 0.7500000000000021094 ) ;
#735 = VECTOR ( 'NONE', #19670, 1000.000000000000000 ) ;
#736 = DIRECTION ( 'NONE',  ( 0.000000000000000000, 1.000000000000000000, 0.000000000000000000 ) ) ;
#737 = DIRECTION ( 'NONE',  ( 3.469446951953614978E-15, 2.999999999999999839E-15, 1.000000000000000000 ) ) ;
#738 = CARTESIAN_POINT ( 'NONE',  ( 44.81606138205700063, 18.19123852234599426, 73.05501292736995822 ) ) ;
#739 = APPLICATION_CONTEXT ( 'automotive_design' ) ;
#740 = CARTESIAN_POINT ( 'NONE',  ( 40.21566563214662438, -6.499520549983879292, 82.71640034338507519 ) ) ;
#741 = CARTESIAN_POINT ( 'NONE',  ( 31.81606138205700418, 38.19123852234599070, 73.05501292736988717 ) ) ;
#742 = EDGE_LOOP ( 'NONE', ( #8248, #22273, #16316, #86 ) ) ;
#743 = CARTESIAN_POINT ( 'NONE',  ( 39.32240756636089429, -21.95458418863069028, 75.30830412695317477 ) ) ;
#744 = LINE ( 'NONE', #10175, #2475 ) ;
#745 = ORIENTED_EDGE ( 'NONE', *, *, #978, .F. ) ;
#746 = ORIENTED_EDGE ( 'NONE', *, *, #3453, .F. ) ;
#747 = CARTESIAN_POINT ( 'NONE',  ( 39.12911128074872380, -15.50384086642191228, 69.06206559358665231 ) ) ;
#748 = ADVANCED_FACE ( 'NONE', ( #710 ), #20321, .F. ) ;
#749 = ADVANCED_FACE ( 'NONE', ( #4354 ), #21994, .F. ) ;
#750 = VECTOR ( 'NONE', #17336, 1000.000000000000227 ) ;
#751 = CARTESIAN_POINT ( 'NONE',  ( 39.82603832034400426, -28.31368208888610027, 72.40698646996131060 ) ) ;
#752 = DIRECTION ( 'NONE',  ( -9.121204216617950752E-31, -0.7071067811865461294, -0.7071067811865490160 ) ) ;
#753 = CARTESIAN_POINT ( 'NONE',  ( 30.81606138205700418, -21.15876147765404625, 76.30501292736998664 ) ) ;
#754 = CARTESIAN_POINT ( 'NONE',  ( 40.31606138205700773, -13.25716901376042323, 21.21736665487721041 ) ) ;
#755 = ORIENTED_EDGE ( 'NONE', *, *, #12133, .T. ) ;
#756 = CARTESIAN_POINT ( 'NONE',  ( 40.30296647725818104, -6.854917929055414305, 82.66861761357043292 ) ) ;
#757 = DIRECTION ( 'NONE',  ( 0.000000000000000000, 0.000000000000000000, -1.000000000000000000 ) ) ;
#758 = EDGE_CURVE ( 'NONE', #12000, #4126, #215, .T. ) ;
#759 = CARTESIAN_POINT ( 'NONE',  ( 36.89935272106204422, -27.21368208888609885, 69.52238214136765748 ) ) ;
#760 = CARTESIAN_POINT ( 'NONE',  ( 43.31606138205700773, -18.80550481115970740, 25.27912300651437150 ) ) ;
#761 = CARTESIAN_POINT ( 'NONE',  ( 33.81606138205700063, 22.19123852234703520, 80.30501292736994401 ) ) ;
#762 = CARTESIAN_POINT ( 'NONE',  ( 38.26194895904383486, -3.013682088886100008, 69.64448340153879258 ) ) ;
#763 = FACE_OUTER_BOUND ( 'NONE', #937, .T. ) ;
#764 = CARTESIAN_POINT ( 'NONE',  ( 37.80618814713140097, -21.91368208888611235, 73.13360434286903455 ) ) ;
#765 = CIRCLE ( 'NONE', #17232, 0.5000000000000004441 ) ;
#766 = CARTESIAN_POINT ( 'NONE',  ( 39.82744760895728575, -21.57196225014778790, 75.82680905536302873 ) ) ;
#767 = ADVANCED_FACE ( 'NONE', ( #6412 ), #16191, .F. ) ;
#768 = DIRECTION ( 'NONE',  ( 0.000000000000000000, -0.4425581086832400257, 0.8967398287344627850 ) ) ;
#769 = VECTOR ( 'NONE', #7198, 1000.000000000000114 ) ;
#770 = CARTESIAN_POINT ( 'NONE',  ( 37.12184278917507640, -26.10384086642191193, 71.32335560751960202 ) ) ;
#771 = CARTESIAN_POINT ( 'NONE',  ( 36.49096545463212493, -13.51368208888610489, 71.43714994484034264 ) ) ;
#772 = LINE ( 'NONE', #24338, #9040 ) ;
#773 = ORIENTED_EDGE ( 'NONE', *, *, #17559, .F. ) ;
#774 = CIRCLE ( 'NONE', #1188, 1.000000000000000888 ) ;
#775 = CARTESIAN_POINT ( 'NONE',  ( 39.82603832034400426, -5.303840866421906775, 70.35351908239857721 ) ) ;
#776 = LINE ( 'NONE', #24468, #17159 ) ;
#777 = CARTESIAN_POINT ( 'NONE',  ( 37.33957961208646736, -3.813682088886109156, 72.81632618279323310 ) ) ;
#778 = EDGE_LOOP ( 'NONE', ( #24874, #9802, #12952, #15567 ) ) ;
#779 = CARTESIAN_POINT ( 'NONE',  ( 40.77203464402485622, -18.51368208888610312, 71.32335560751960202 ) ) ;
#780 = ORIENTED_EDGE ( 'NONE', *, *, #14281, .T. ) ;
#781 = DIRECTION ( 'NONE',  ( 0.000000000000000000, -1.000000000000000000, 0.000000000000000000 ) ) ;
#782 = DIRECTION ( 'NONE',  ( -1.000000000000000000, -2.999999999999999839E-15, 0.000000000000000000 ) ) ;
#783 = CARTESIAN_POINT ( 'NONE',  ( 39.41296390513587511, -11.20384086642191335, 71.08074471024443142 ) ) ;
#784 = AXIS2_PLACEMENT_3D ( 'NONE', #8790, #6837, #14690 ) ;
#785 = FACE_OUTER_BOUND ( 'NONE', #18859, .T. ) ;
#786 = VERTEX_POINT ( 'NONE', #6157 ) ;
#787 = DIRECTION ( 'NONE',  ( 0.000000000000000000, 1.861251128379125107E-14, 1.000000000000000000 ) ) ;
#788 = B_SPLINE_CURVE_WITH_KNOTS ( 'NONE', 3,
 ( #10750, #931, #8822, #10874 ),
 .UNSPECIFIED., .F., .F.,
 ( 4, 4 ),
 ( 0.000000000000000000, 1.000000000000000000 ),
 .UNSPECIFIED. ) ;
#789 = DIRECTION ( 'NONE',  ( 9.614242282381077875E-31, 0.7071067811865460184, 0.7071067811865489050 ) ) ;
#790 = CARTESIAN_POINT ( 'NONE',  ( 39.73277004305197124, -19.40384086642191264, 69.52238214136768590 ) ) ;
#791 = CIRCLE ( 'NONE', #19318, 2.000000000000001776 ) ;
#792 = CARTESIAN_POINT ( 'NONE',  ( 33.31606138205700773, -27.17722769842920272, 59.42551550655435477 ) ) ;
#793 = CARTESIAN_POINT ( 'NONE',  ( 37.33957961208646736, -27.81368208888611093, 72.81632618279320468 ) ) ;
#794 = LINE ( 'NONE', #9887, #17878 ) ;
#795 = FACE_OUTER_BOUND ( 'NONE', #17917, .T. ) ;
#796 = EDGE_CURVE ( 'NONE', #6775, #12825, #1233, .T. ) ;
#797 = VECTOR ( 'NONE', #6910, 1000.000000000000000 ) ;
#798 = ORIENTED_EDGE ( 'NONE', *, *, #889, .T. ) ;
#799 = EDGE_CURVE ( 'NONE', #12627, #3377, #20490, .T. ) ;
#800 = FACE_OUTER_BOUND ( 'NONE', #1702, .T. ) ;
#801 = DIRECTION ( 'NONE',  ( 1.444147469618246167E-16, -0.8212051873014210024, -0.5706330172266920187 ) ) ;
#802 = EDGE_CURVE ( 'NONE', #973, #13467, #6103, .T. ) ;
#803 = CARTESIAN_POINT ( 'NONE',  ( 38.26194895904384907, -14.60384086642191548, 73.11602215082116629 ) ) ;
#804 = CARTESIAN_POINT ( 'NONE',  ( 0.000000000000000000, 0.000000000000000000, 0.000000000000000000 ) ) ;
#805 = LINE ( 'NONE', #8691, #16582 ) ;
#806 = DIRECTION ( 'NONE',  ( -1.000000000000000000, 0.000000000000000000, 2.478176394252580155E-16 ) ) ;
#807 = PLANE ( 'NONE',  #2853 ) ;
#808 = CARTESIAN_POINT ( 'NONE',  ( 38.00113996487112189, 0.2961591335780902612, 70.22690120949094705 ) ) ;
#809 = CARTESIAN_POINT ( 'NONE',  ( 46.81606138205702194, -20.48383445069734066, 23.59578481461660004 ) ) ;
#810 = ORIENTED_EDGE ( 'NONE', *, *, #4809, .T. ) ;
#811 = VECTOR ( 'NONE', #1544, 1000.000000000000000 ) ;
#812 = EDGE_CURVE ( 'NONE', #17171, #21810, #20825, .T. ) ;
#813 = CARTESIAN_POINT ( 'NONE',  ( 39.82603832034400426, -26.31368208888611093, 72.40698646996131060 ) ) ;
#814 = ORIENTED_EDGE ( 'NONE', *, *, #2858, .T. ) ;
#815 = ORIENTED_EDGE ( 'NONE', *, *, #8639, .F. ) ;
#816 = CARTESIAN_POINT ( 'NONE',  ( 42.99361969242278292, 2.839052459004266726, 6.102834979010582472 ) ) ;
#817 = CARTESIAN_POINT ( 'NONE',  ( 43.24475484328152675, -1.357181138186998925, 80.05501292736997243 ) ) ;
#818 = VECTOR ( 'NONE', #17657, 1000.000000000000114 ) ;
#819 = CARTESIAN_POINT ( 'NONE',  ( 38.26194895904384197, -28.60384086642191193, 72.51602215082114355 ) ) ;
#820 = CARTESIAN_POINT ( 'NONE',  ( 38.73920764526925353, 1.886317911113897905, 72.49843995877333214 ) ) ;
#821 = VERTEX_POINT ( 'NONE', #16699 ) ;
#822 = ORIENTED_EDGE ( 'NONE', *, *, #5627, .F. ) ;
#823 = CARTESIAN_POINT ( 'NONE',  ( 36.31606138205700063, 8.691238522346989015, 65.80501292736998664 ) ) ;
#824 = DIRECTION ( 'NONE',  ( 0.000000000000000000, -1.000000000000000000, 2.999999999999999839E-15 ) ) ;
#825 = CARTESIAN_POINT ( 'NONE',  ( 37.33957961208645315, -13.80384086642190766, 69.94417936956672577 ) ) ;
#826 = CARTESIAN_POINT ( 'NONE',  ( 31.81606138205700418, -34.55876147765401640, 70.30501292737011454 ) ) ;
#827 = EDGE_LOOP ( 'NONE', ( #8817, #12206, #569, #6532 ) ) ;
#828 = VERTEX_POINT ( 'NONE', #10781 ) ;
#829 = ORIENTED_EDGE ( 'NONE', *, *, #19452, .F. ) ;
#830 = DIRECTION ( 'NONE',  ( -1.734723475976809806E-16, 0.000000000000000000, -1.000000000000000000 ) ) ;
#831 = AXIS2_PLACEMENT_3D ( 'NONE', #7687, #10004, #9635 ) ;
#832 = CARTESIAN_POINT ( 'NONE',  ( 36.68196826583682935, -7.613682088886103649, 71.96809898377890136 ) ) ;
#833 = DIRECTION ( 'NONE',  ( 0.000000000000000000, -0.8212051873014208914, -0.5706330172266919076 ) ) ;
#834 = LINE ( 'NONE', #10778, #14932 ) ;
#835 = VECTOR ( 'NONE', #10940, 1000.000000000000000 ) ;
#836 = CARTESIAN_POINT ( 'NONE',  ( 31.81606138205700418, -34.55876147765410167, 66.30501292737000085 ) ) ;
#837 = DIRECTION ( 'NONE',  ( -1.000000000000000000, 1.115179377413661005E-30, 3.717264591378870232E-16 ) ) ;
#838 = CARTESIAN_POINT ( 'NONE',  ( 36.58819418470650220, -6.140949260442095436, 82.76158051492357970 ) ) ;
#839 = EDGE_CURVE ( 'NONE', #20815, #9471, #19260, .T. ) ;
#840 = CARTESIAN_POINT ( 'NONE',  ( 43.23147868389327897, 41.90149715599300606, 79.37823623207322044 ) ) ;
#841 = ORIENTED_EDGE ( 'NONE', *, *, #2654, .F. ) ;
#842 = ORIENTED_EDGE ( 'NONE', *, *, #1376, .F. ) ;
#843 = CARTESIAN_POINT ( 'NONE',  ( 40.31606138205700063, 8.691238522346987239, 65.30501292736998664 ) ) ;
#844 = CARTESIAN_POINT ( 'NONE',  ( 36.07789103942398867, -27.41368208888610525, 70.70992431699450265 ) ) ;
#846 = VECTOR ( 'NONE', #7817, 1000.000000000000000 ) ;
#845 = CARTESIAN_POINT ( 'NONE',  ( 39.51027997493896748, -16.51368208888610312, 71.32335560751960202 ) ) ;
#847 = ORIENTED_EDGE ( 'NONE', *, *, #24054, .T. ) ;
#848 = VERTEX_POINT ( 'NONE', #18891 ) ;
#849 = CYLINDRICAL_SURFACE ( 'NONE', #21888, 1.000000000000000888 ) ;
#850 = CARTESIAN_POINT ( 'NONE',  ( 40.14115730948191185, -4.513682088886103116, 71.32335560751961623 ) ) ;
#851 = CARTESIAN_POINT ( 'NONE',  ( 39.51027997493896748, -1.103840866421911704, 71.43714994484034264 ) ) ;
#852 = AXIS2_PLACEMENT_3D ( 'NONE', #7427, #17477, #15521 ) ;
#853 = LINE ( 'NONE', #22510, #16556 ) ;
#854 = CARTESIAN_POINT ( 'NONE',  ( 36.98690846071097837, -5.813682088886107380, 73.30173637941818754 ) ) ;
#855 = DIRECTION ( 'NONE',  ( 1.000000000000000000, -0.000000000000000000, 0.000000000000000000 ) ) ;
#856 = DIRECTION ( 'NONE',  ( 0.000000000000000000, 0.000000000000000000, -1.000000000000000000 ) ) ;
#857 = DIRECTION ( 'NONE',  ( -1.734723475976879818E-16, 1.000000000000000000, -4.343580702399009298E-14 ) ) ;
#858 = DIRECTION ( 'NONE',  ( 0.000000000000000000, 2.999999999999999839E-15, 1.000000000000000000 ) ) ;
#859 = DIRECTION ( 'NONE',  ( 0.000000000000000000, -6.938893903907222067E-15, -1.000000000000000000 ) ) ;
#860 = CYLINDRICAL_SURFACE ( 'NONE', #7319, 0.4999999999999998890 ) ;
#861 = B_SPLINE_CURVE_WITH_KNOTS ( 'NONE', 3,
 ( #25078, #7720, #7463, #19426 ),
 .UNSPECIFIED., .F., .F.,
 ( 4, 4 ),
 ( 0.000000000000000000, 1.000000000000000000 ),
 .UNSPECIFIED. ) ;
#862 = AXIS2_PLACEMENT_3D ( 'NONE', #7436, #23134, #19536 ) ;
#863 = CARTESIAN_POINT ( 'NONE',  ( 31.91606138205697363, -3.929900956088018038, -7.102449327239662935 ) ) ;
#864 = ORIENTED_EDGE ( 'NONE', *, *, #11208, .F. ) ;
#865 = CARTESIAN_POINT ( 'NONE',  ( 40.26527270485448184, -20.73887650502739177, 75.40739922272783247 ) ) ;
#866 = ADVANCED_FACE ( 'NONE', ( #9118 ), #22748, .T. ) ;
#867 = CARTESIAN_POINT ( 'NONE',  ( 42.96606138205694236, 5.208890205473748480, 5.429380561359602453 ) ) ;
#868 = VERTEX_POINT ( 'NONE', #20952 ) ;
#869 = ORIENTED_EDGE ( 'NONE', *, *, #6116, .T. ) ;
#870 = CARTESIAN_POINT ( 'NONE',  ( 40.26954217208372455, -18.90384086642191619, 72.86986841596734621 ) ) ;
#871 = CARTESIAN_POINT ( 'NONE',  ( 39.75915168707250302, -18.71368208888610241, 70.26145752964251301 ) ) ;
#872 = DIRECTION ( 'NONE',  ( 1.000000000000000000, -0.000000000000000000, 0.000000000000000000 ) ) ;
#873 = CARTESIAN_POINT ( 'NONE',  ( 40.31606138205700773, -12.40281258615395821, 20.95421293576468358 ) ) ;
#874 = VERTEX_POINT ( 'NONE', #24530 ) ;
#875 = DIRECTION ( 'NONE',  ( 3.491481338843135327E-15, 1.000000000000000000, -3.000000000000000628E-15 ) ) ;
#876 = PLANE ( 'NONE',  #7170 ) ;
#877 = CARTESIAN_POINT ( 'NONE',  ( 40.26954217208371034, -28.71368208888610241, 69.89063713639254161 ) ) ;
#878 = CIRCLE ( 'NONE', #9556, 2.000000000000000888 ) ;
#879 = ORIENTED_EDGE ( 'NONE', *, *, #18939, .T. ) ;
#880 = CIRCLE ( 'NONE', #9142, 1.000000000000000888 ) ;
#881 = EDGE_CURVE ( 'NONE', #23679, #25358, #20565, .T. ) ;
#882 = FACE_OUTER_BOUND ( 'NONE', #20497, .T. ) ;
#883 = CYLINDRICAL_SURFACE ( 'NONE', #73, 1.499999999999999778 ) ;
#884 = CARTESIAN_POINT ( 'NONE',  ( 40.14115730948191185, 1.486317911113896884, 71.32335560751963044 ) ) ;
#885 = DIRECTION ( 'NONE',  ( 0.000000000000000000, 0.000000000000000000, -1.000000000000000000 ) ) ;
#886 = ADVANCED_FACE ( 'NONE', ( #3294 ), #4978, .F. ) ;
#887 = AXIS2_PLACEMENT_3D ( 'NONE', #14310, #8262, #20232 ) ;
#888 = CARTESIAN_POINT ( 'NONE',  ( 36.87297107704153376, -17.71368208888610951, 72.49904802271740323 ) ) ;
#889 = EDGE_CURVE ( 'NONE', #2214, #17745, #3160, .T. ) ;
#890 = EDGE_CURVE ( 'NONE', #20252, #9149, #6911, .T. ) ;
#891 = EDGE_CURVE ( 'NONE', #14769, #4753, #6782, .T. ) ;
#892 = CARTESIAN_POINT ( 'NONE',  ( 43.81606138205700063, -27.52349462642295208, 56.67559192035834315 ) ) ;
#893 = DIRECTION ( 'NONE',  ( -1.000000000000000000, 0.000000000000000000, 0.000000000000000000 ) ) ;
#894 = CARTESIAN_POINT ( 'NONE',  ( 39.41296390513587511, -17.20384086642191335, 71.08074471024441721 ) ) ;
#895 = CARTESIAN_POINT ( 'NONE',  ( 38.37017380507020192, -4.013682088886107557, 73.11602215082118050 ) ) ;
#896 = ORIENTED_EDGE ( 'NONE', *, *, #24579, .T. ) ;
#897 = CARTESIAN_POINT ( 'NONE',  ( 33.31606138205700773, -2.088476903695762665, 19.19551655256602984 ) ) ;
#898 = EDGE_CURVE ( 'NONE', #1130, #12932, #2769, .T. ) ;
#899 = ORIENTED_EDGE ( 'NONE', *, *, #20502, .F. ) ;
#900 = EDGE_CURVE ( 'NONE', #13184, #17478, #14637, .T. ) ;
#901 = AXIS2_PLACEMENT_3D ( 'NONE', #10296, #24061, #6178 ) ;
#902 = CARTESIAN_POINT ( 'NONE',  ( 38.26194895904384907, -4.603840866421914590, 73.11602215082118050 ) ) ;
#903 = FACE_BOUND ( 'NONE', #23651, .T. ) ;
#904 = VECTOR ( 'NONE', #2124, 1000.000000000000000 ) ;
#905 = CARTESIAN_POINT ( 'NONE',  ( 36.49096545463212493, -3.513682088886103116, 71.43714994484035685 ) ) ;
#906 = ORIENTED_EDGE ( 'NONE', *, *, #891, .T. ) ;
#907 = CARTESIAN_POINT ( 'NONE',  ( 37.50301148336529167, -9.113682088886102761, 69.06206559358666652 ) ) ;
#908 = ORIENTED_EDGE ( 'NONE', *, *, #22325, .F. ) ;
#909 = CARTESIAN_POINT ( 'NONE',  ( 39.81606138205700063, -1.383222575549920119, 62.14461230196212682 ) ) ;
#910 = CARTESIAN_POINT ( 'NONE',  ( 39.51027997493896748, -13.10384086642191015, 71.43714994484032843 ) ) ;
#911 = CARTESIAN_POINT ( 'NONE',  ( 43.81606138205700063, -24.55876147765401996, 67.80501292737008612 ) ) ;
#912 = ADVANCED_FACE ( 'NONE', ( #16562 ), #11803, .T. ) ;
#913 = ORIENTED_EDGE ( 'NONE', *, *, #13102, .T. ) ;
#914 = VECTOR ( 'NONE', #23046, 1000.000000000000000 ) ;
#915 = CYLINDRICAL_SURFACE ( 'NONE', #21603, 3.000000000000000444 ) ;
#916 = CARTESIAN_POINT ( 'NONE',  ( 32.81606138205700773, 38.19123852234599070, 72.05501292736988717 ) ) ;
#917 = CARTESIAN_POINT ( 'NONE',  ( 35.86008812008917346, -14.10384086642191548, 71.32335560751961623 ) ) ;
#918 = CIRCLE ( 'NONE', #18590, 0.9999999999999937828 ) ;
#919 = CARTESIAN_POINT ( 'NONE',  ( 38.18494427818247061, -22.22127907754186893, 75.81001292736998209 ) ) ;
#920 = CARTESIAN_POINT ( 'NONE',  ( 38.37017380507020192, -20.01368208888610667, 73.11602215082116629 ) ) ;
#921 = CYLINDRICAL_SURFACE ( 'NONE', #3999, 1.100000000000000311 ) ;
#922 = VECTOR ( 'NONE', #13989, 1000.000000000000114 ) ;
#923 = DIRECTION ( 'NONE',  ( 2.690219486203388234E-15, -0.8967398287344627850, -0.4425581086832399147 ) ) ;
#924 = VECTOR ( 'NONE', #10529, 1000.000000000000000 ) ;
#925 = ORIENTED_EDGE ( 'NONE', *, *, #22452, .T. ) ;
#926 = DIRECTION ( 'NONE',  ( 0.000000000000000000, 0.8212051873014208914, 0.5706330172266919076 ) ) ;
#927 = LINE ( 'NONE', #12805, #16343 ) ;
#928 = VECTOR ( 'NONE', #2718, 1000.000000000000000 ) ;
#929 = CARTESIAN_POINT ( 'NONE',  ( 38.82593461698264292, -14.70384086642191690, 73.13360434286903455 ) ) ;
#930 = DIRECTION ( 'NONE',  ( 1.000000000000000000, 0.000000000000000000, 0.000000000000000000 ) ) ;
#931 = CARTESIAN_POINT ( 'NONE',  ( 33.56669025312649524, 3.416671603466172602, 6.349359658337577983 ) ) ;
#932 = LINE ( 'NONE', #675, #6543 ) ;
#933 = AXIS2_PLACEMENT_3D ( 'NONE', #16052, #8463, #9892 ) ;
#934 = CARTESIAN_POINT ( 'NONE',  ( 30.81606138205700418, 34.87886987267149408, 80.75501292736984738 ) ) ;
#935 = CARTESIAN_POINT ( 'NONE',  ( 39.38009889167648936, -25.40384086642190908, 70.00779233799262613 ) ) ;
#936 = DIRECTION ( 'NONE',  ( 1.734723475976805122E-15, 2.999999999999999839E-15, 1.000000000000000000 ) ) ;
#937 = EDGE_LOOP ( 'NONE', ( #6127, #19955, #5649, #11614 ) ) ;
#938 = AXIS2_PLACEMENT_3D ( 'NONE', #817, #24387, #22469 ) ;
#939 = CARTESIAN_POINT ( 'NONE',  ( 38.82593461698262871, -22.91368208888609459, 69.62690120949091011 ) ) ;
#940 = ORIENTED_EDGE ( 'NONE', *, *, #8964, .T. ) ;
#941 = EDGE_LOOP ( 'NONE', ( #3944, #19997, #17589, #15115 ) ) ;
#942 = FACE_OUTER_BOUND ( 'NONE', #19532, .T. ) ;
#943 = AXIS2_PLACEMENT_3D ( 'NONE', #9955, #8026, #8404 ) ;
#944 = CARTESIAN_POINT ( 'NONE',  ( 36.31606138205700063, -31.05876147765400574, 73.55501292737010033 ) ) ;
#945 = CARTESIAN_POINT ( 'NONE',  ( 37.31647492878122563, 0.6863179111138985045, 70.72433947564853440 ) ) ;
#946 = CARTESIAN_POINT ( 'NONE',  ( 39.31564783533279694, -29.30384086642190766, 70.72433947564850598 ) ) ;
#947 = VERTEX_POINT ( 'NONE', #19641 ) ;
#948 = ORIENTED_EDGE ( 'NONE', *, *, #22550, .T. ) ;
#949 = DIRECTION ( 'NONE',  ( -1.000000000000000000, 0.000000000000000000, 0.000000000000000000 ) ) ;
#950 = VECTOR ( 'NONE', #22281, 1000.000000000000000 ) ;
#951 = FACE_OUTER_BOUND ( 'NONE', #1705, .T. ) ;
#952 = VERTEX_POINT ( 'NONE', #19387 ) ;
#953 = DIRECTION ( 'NONE',  ( -1.000000000000000000, -2.999999999999999839E-15, 0.000000000000000000 ) ) ;
#954 = CARTESIAN_POINT ( 'NONE',  ( 39.38009889167648936, -3.403840866421908196, 70.00779233799264034 ) ) ;
#955 = FACE_OUTER_BOUND ( 'NONE', #12125, .T. ) ;
#956 = VECTOR ( 'NONE', #7416, 1000.000000000000114 ) ;
#957 = CARTESIAN_POINT ( 'NONE',  ( 30.81606138205700418, -1.357181138186998925, 79.30501292737000085 ) ) ;
#958 = ORIENTED_EDGE ( 'NONE', *, *, #16247, .F. ) ;
#959 = ORIENTED_EDGE ( 'NONE', *, *, #4050, .T. ) ;
#960 = ORIENTED_EDGE ( 'NONE', *, *, #16869, .T. ) ;
#961 = CARTESIAN_POINT ( 'NONE',  ( 43.81606138205700063, 36.92314894770294131, 81.17823623207323180 ) ) ;
#962 = CARTESIAN_POINT ( 'NONE',  ( 38.26194895904383486, -1.013682088886101784, 69.64448340153879258 ) ) ;
#963 = CARTESIAN_POINT ( 'NONE',  ( 35.31606138205700773, 3.043703737701412226, 64.67489359404071081 ) ) ;
#964 = AXIS2_PLACEMENT_3D ( 'NONE', #21763, #4252, #7865 ) ;
#965 = FACE_OUTER_BOUND ( 'NONE', #17968, .T. ) ;
#966 = CARTESIAN_POINT ( 'NONE',  ( 43.06606138205700063, 41.44123852234595518, 61.30501292736988006 ) ) ;
#967 = CIRCLE ( 'NONE', #4280, 0.4999999999999994449 ) ;
#968 = CARTESIAN_POINT ( 'NONE',  ( 31.81606138205700418, 18.19123852234598715, 71.05501292736995822 ) ) ;
#969 = CARTESIAN_POINT ( 'NONE',  ( 28.84183937708599998, -36.05761098950961241, 70.36375082663613512 ) ) ;
#970 = CARTESIAN_POINT ( 'NONE',  ( 33.31606138205700773, 3.392460599465057403, 64.84545171350526971 ) ) ;
#971 = SHAPE_REPRESENTATION_RELATIONSHIP ( 'NONE' , 'NONE' ,  #9445, #19676 ) ;
#972 = CARTESIAN_POINT ( 'NONE',  ( 35.14099152588522657, -10.60718113818700026, 83.30501292737001506 ) ) ;
#973 = VERTEX_POINT ( 'NONE', #15403 ) ;
#974 = ORIENTED_EDGE ( 'NONE', *, *, #19644, .F. ) ;
#976 = ADVANCED_FACE ( 'NONE', ( #13727 ), #1722, .T. ) ;
#975 = DIRECTION ( 'NONE',  ( -1.000000000000000000, 0.000000000000000000, 1.734723475976804876E-16 ) ) ;
#977 = DIRECTION ( 'NONE',  ( 0.000000000000000000, 1.000000000000000000, 0.000000000000000000 ) ) ;
#978 = EDGE_CURVE ( 'NONE', #13410, #10587, #1600, .T. ) ;
#979 = MECHANICAL_DESIGN_GEOMETRIC_PRESENTATION_REPRESENTATION (  '', ( #16209 ), #14965 ) ;
#980 = CARTESIAN_POINT ( 'NONE',  ( 37.60469502381300089, -15.21368208888610063, 70.49320253461759478 ) ) ;
#981 = VERTEX_POINT ( 'NONE', #23370 ) ;
#982 = ORIENTED_EDGE ( 'NONE', *, *, #6042, .T. ) ;
#983 = CARTESIAN_POINT ( 'NONE',  ( 44.06606138205700063, 40.39281886181299797, 82.55501292736983032 ) ) ;
#984 = CARTESIAN_POINT ( 'NONE',  ( 39.29254315202756231, -2.813682088886101162, 69.94417936956673998 ) ) ;
#985 = CARTESIAN_POINT ( 'NONE',  ( 39.38009889167648936, -21.40384086642190553, 70.00779233799262613 ) ) ;
#986 = VECTOR ( 'NONE', #18996, 1000.000000000000000 ) ;
#987 = CIRCLE ( 'NONE', #1749, 1.000000000000000888 ) ;
#988 = DIRECTION ( 'NONE',  ( -4.040217218240261171E-16, -0.4425581086832399702, 0.8967398287344627850 ) ) ;
#989 = VECTOR ( 'NONE', #18459, 1000.000000000000000 ) ;
#990 = CARTESIAN_POINT ( 'NONE',  ( 39.64521430340304420, -10.81368208888610027, 69.45876917294177133 ) ) ;
#992 = ORIENTED_EDGE ( 'NONE', *, *, #12189, .F. ) ;
#991 = DIRECTION ( 'NONE',  ( -4.625929269271484533E-15, 0.8967398287344634511, 0.4425581086832385824 ) ) ;
#993 = DIRECTION ( 'NONE',  ( 7.071067811865491110E-16, -0.9008287146801832179, 0.4341746501209495790 ) ) ;
#994 = EDGE_CURVE ( 'NONE', #25303, #14052, #9742, .T. ) ;
#995 = FACE_BOUND ( 'NONE', #20971, .T. ) ;
#996 = CARTESIAN_POINT ( 'NONE',  ( 44.81606138205700063, -30.95005513552129983, 81.04249030099066431 ) ) ;
#997 = PRODUCT_DEFINITION_FORMATION_WITH_SPECIFIED_SOURCE ( 'ANY', '', #19806, .NOT_KNOWN. ) ;
#998 = CARTESIAN_POINT ( 'NONE',  ( 43.06468080341912241, 3.415100481987971115, 6.350457055188933886 ) ) ;
#999 = FACE_OUTER_BOUND ( 'NONE', #16254, .T. ) ;
#1000 = VECTOR ( 'NONE', #20638, 1000.000000000000000 ) ;
#1001 = CARTESIAN_POINT ( 'NONE',  ( 35.81606138205700063, 9.191238522346999673, 69.30501292736997243 ) ) ;
#1002 = VERTEX_POINT ( 'NONE', #21585 ) ;
#1003 = DIRECTION ( 'NONE',  ( 0.000000000000000000, 1.000000000000000000, 0.000000000000000000 ) ) ;
#1004 = CARTESIAN_POINT ( 'NONE',  ( 32.81606138205700773, -27.11289203277224402, 56.96090842897168471 ) ) ;
#1005 = ORIENTED_EDGE ( 'NONE', *, *, #20302, .F. ) ;
#1006 = AXIS2_PLACEMENT_3D ( 'NONE', #18778, #9324, #5440 ) ;
#1007 = ORIENTED_EDGE ( 'NONE', *, *, #15153, .F. ) ;
#1008 = CARTESIAN_POINT ( 'NONE',  ( 38.26194895904384197, -16.60384086642191548, 73.71602215082113219 ) ) ;
#1009 = CARTESIAN_POINT ( 'NONE',  ( 36.87297107704152666, -21.71368208888610951, 72.49904802271740323 ) ) ;
#1010 = CARTESIAN_POINT ( 'NONE',  ( 40.31606138205700773, 37.94123852234599781, 74.30501292736988717 ) ) ;
#1011 = LINE ( 'NONE', #8894, #24974 ) ;
#1012 = EDGE_LOOP ( 'NONE', ( #18298, #22187, #18869, #14295 ) ) ;
#1013 = CARTESIAN_POINT ( 'NONE',  ( 38.14273442609844977, 37.69123852234599781, 70.32014858831708182 ) ) ;
#1014 = CARTESIAN_POINT ( 'NONE',  ( 31.81606138205700418, 44.92314894770294131, 80.37823623207322044 ) ) ;
#1015 = CARTESIAN_POINT ( 'NONE',  ( 36.36258059203031934, -25.71368208888611306, 72.86986841596734621 ) ) ;
#1016 = VECTOR ( 'NONE', #24571, 1000.000000000000000 ) ;
#1017 = EDGE_LOOP ( 'NONE', ( #16280, #22526, #11907, #24276 ) ) ;
#1018 =( LENGTH_UNIT ( ) NAMED_UNIT ( * ) SI_UNIT ( .MILLI., .METRE. ) );
#1019 = DIRECTION ( 'NONE',  ( -1.000000000000000000, 0.000000000000000000, 0.000000000000000000 ) ) ;
#1020 = CARTESIAN_POINT ( 'NONE',  ( 39.98359781491296161, -2.413682088886103472, 71.86517103874048473 ) ) ;
#1021 = PLANE ( 'NONE',  #24911 ) ;
#1022 = EDGE_CURVE ( 'NONE', #11745, #2525, #15272, .T. ) ;
#1023 = CARTESIAN_POINT ( 'NONE',  ( 38.93415946300898867, -22.11368208888610454, 73.09843995877329803 ) ) ;
#1024 = CARTESIAN_POINT ( 'NONE',  ( 39.32240756636089429, -21.96791893307624832, 75.80813956697402034 ) ) ;
#1025 = FACE_OUTER_BOUND ( 'NONE', #16753, .T. ) ;
#1026 = CARTESIAN_POINT ( 'NONE',  ( 38.37017380507018771, -17.60384086642191193, 70.24448340153875847 ) ) ;
#1027 = CARTESIAN_POINT ( 'NONE',  ( 38.93415946300897446, -6.113682088886107202, 73.09843995877331224 ) ) ;
#1028 = ORIENTED_EDGE ( 'NONE', *, *, #24774, .T. ) ;
#1029 = LINE ( 'NONE', #18695, #10688 ) ;
#1030 = VERTEX_POINT ( 'NONE', #25162 ) ;
#1031 = CARTESIAN_POINT ( 'NONE',  ( 36.68196826583682935, -4.003840866421911393, 70.79240656858108593 ) ) ;
#1032 = ADVANCED_FACE ( 'NONE', ( #7804 ), #17472, .F. ) ;
#1033 = CARTESIAN_POINT ( 'NONE',  ( 38.31606138205700063, -30.30876147765400574, 72.30501292737010033 ) ) ;
#1034 = ADVANCED_FACE ( 'NONE', ( #7294 ), #7553, .T. ) ;
#1035 = CARTESIAN_POINT ( 'NONE',  ( 39.95015449827720744, -8.613682088886104538, 70.79240656858107172 ) ) ;
#1036 = EDGE_LOOP ( 'NONE', ( #23616, #23189, #2368, #21937 ) ) ;
#1037 = CARTESIAN_POINT ( 'NONE',  ( 35.86008812008917346, -9.513682088886103116, 71.43714994484035685 ) ) ;
#1038 = EDGE_LOOP ( 'NONE', ( #11997, #17760, #10721, #8351 ) ) ;
#1039 = CARTESIAN_POINT ( 'NONE',  ( 41.31606138205700063, 8.104266321858618838, 55.82104096753806033 ) ) ;
#1040 = EDGE_CURVE ( 'NONE', #24026, #19555, #16326, .T. ) ;
#1041 = CARTESIAN_POINT ( 'NONE',  ( 39.37952058850012804, -13.00384086642191228, 71.78268878715390144 ) ) ;
#1042 = EDGE_CURVE ( 'NONE', #9104, #4853, #5608, .T. ) ;
#1043 = ADVANCED_FACE ( 'NONE', ( #13603 ), #21202, .T. ) ;
#1044 = DIRECTION ( 'NONE',  ( 1.000000000000000000, -0.000000000000000000, 0.000000000000000000 ) ) ;
#1045 = ORIENTED_EDGE ( 'NONE', *, *, #24087, .F. ) ;
#1046 = DIRECTION ( 'NONE',  ( -2.727049986597863807E-15, 0.7516416929448760387, 0.6595716529892418079 ) ) ;
#1047 = LINE ( 'NONE', #4925, #6305 ) ;
#1048 = CARTESIAN_POINT ( 'NONE',  ( 36.36258059203030513, -17.90384086642190908, 69.89063713639259845 ) ) ;
#1049 = FACE_OUTER_BOUND ( 'NONE', #24533, .T. ) ;
#1050 = CARTESIAN_POINT ( 'NONE',  ( 44.81606138205700063, -24.55876147765401285, 70.30501292737008612 ) ) ;
#1051 = CARTESIAN_POINT ( 'NONE',  ( 39.98359781491296161, -20.41368208888610525, 71.86517103874047052 ) ) ;
#1052 = DIRECTION ( 'NONE',  ( -2.011972697750612571E-15, 0.6595716529892353686, -0.7516416929448815898 ) ) ;
#1053 = ADVANCED_FACE ( 'NONE', ( #5490 ), #11680, .T. ) ;
#1054 = DIRECTION ( 'NONE',  ( 0.000000000000000000, -0.3299742535181005021, 0.9439899321577387425 ) ) ;
#1055 = ORIENTED_EDGE ( 'NONE', *, *, #5647, .F. ) ;
#1056 = CARTESIAN_POINT ( 'NONE',  ( 43.23147868389327897, 41.67000142393845152, 79.57823623207323749 ) ) ;
#1057 = DIRECTION ( 'NONE',  ( 0.000000000000000000, -3.469446951953613400E-15, -1.000000000000000000 ) ) ;
#1058 = CARTESIAN_POINT ( 'NONE',  ( 40.14115730948191185, -15.10384086642191015, 71.43714994484031422 ) ) ;
#1059 = DIRECTION ( 'NONE',  ( 0.000000000000000000, 0.000000000000000000, 1.000000000000000000 ) ) ;
#1060 = DIRECTION ( 'NONE',  ( 0.000000000000000000, -9.251858538542962756E-15, -1.000000000000000000 ) ) ;
#1061 = CARTESIAN_POINT ( 'NONE',  ( 36.87297107704152666, -27.71368208888610241, 72.49904802271738902 ) ) ;
#1062 = DIRECTION ( 'NONE',  ( -9.925461516413221718E-16, 0.8967398287344632291, 0.4425581086832394151 ) ) ;
#1063 = CARTESIAN_POINT ( 'NONE',  ( 39.38009889167648936, -27.40384086642190908, 70.00779233799262613 ) ) ;
#1064 = CARTESIAN_POINT ( 'NONE',  ( 36.31606138205700063, -20.44477830400171570, 75.97174273075597739 ) ) ;
#1065 = CARTESIAN_POINT ( 'NONE',  ( 39.75915168707250302, -22.71368208888610241, 70.26145752964251301 ) ) ;
#1066 = ORIENTED_EDGE ( 'NONE', *, *, #22005, .T. ) ;
#1067 = ORIENTED_EDGE ( 'NONE', *, *, #19250, .F. ) ;
#1068 = DIRECTION ( 'NONE',  ( 1.000000000000000000, -0.000000000000000000, 0.000000000000000000 ) ) ;
#1069 = FACE_OUTER_BOUND ( 'NONE', #1734, .T. ) ;
#1070 = CARTESIAN_POINT ( 'NONE',  ( 38.26194895904383486, -1.013682088886101784, 70.24448340153877268 ) ) ;
#1071 = ADVANCED_FACE ( 'NONE', ( #3542 ), #22998, .F. ) ;
#1072 = EDGE_CURVE ( 'NONE', #3879, #7931, #5868, .T. ) ;
#1073 = CARTESIAN_POINT ( 'NONE',  ( 37.60469502381300089, -1.213682088886100630, 70.49320253461759478 ) ) ;
#1074 = EDGE_LOOP ( 'NONE', ( #6439, #18112, #14922, #14485 ) ) ;
#1075 = VERTEX_POINT ( 'NONE', #13231 ) ;
#1076 = CARTESIAN_POINT ( 'NONE',  ( 41.06606138205700063, -13.51824891481308910, 37.72654391001022134 ) ) ;
#1077 = DIRECTION ( 'NONE',  ( -4.625929269271484533E-15, 0.8967398287344634511, 0.4425581086832385824 ) ) ;
#1078 = FILL_AREA_STYLE_COLOUR ( '', #9416 ) ;
#1079 = CARTESIAN_POINT ( 'NONE',  ( 37.80618814713138676, -5.703840866421908018, 69.62690120949091011 ) ) ;
#1080 = LINE ( 'NONE', #15257, #5531 ) ;
#1081 = EDGE_CURVE ( 'NONE', #11722, #2503, #12273, .T. ) ;
#1082 = FACE_OUTER_BOUND ( 'NONE', #2152, .T. ) ;
#1083 = ORIENTED_EDGE ( 'NONE', *, *, #18532, .F. ) ;
#1084 = ORIENTED_EDGE ( 'NONE', *, *, #10520, .F. ) ;
#1085 = VERTEX_POINT ( 'NONE', #2756 ) ;
#1086 = DIRECTION ( 'NONE',  ( -1.000000000000000000, 5.510910596163088391E-31, 1.836970198721029688E-16 ) ) ;
#1087 = CARTESIAN_POINT ( 'NONE',  ( 36.64852494920107517, -1.413682088886102806, 70.89533451361948835 ) ) ;
#1088 = FACE_OUTER_BOUND ( 'NONE', #12606, .T. ) ;
#1089 =( NAMED_UNIT ( * ) SI_UNIT ( $, .STERADIAN. ) SOLID_ANGLE_UNIT ( ) );
#1090 = CARTESIAN_POINT ( 'NONE',  ( 42.56606138205700063, -32.75315594507191008, 59.38245422252773409 ) ) ;
#1091 = CARTESIAN_POINT ( 'NONE',  ( 44.31606138205700063, 10.06218483883314718, 67.80501292737497465 ) ) ;
#1092 = EDGE_CURVE ( 'NONE', #467, #5442, #24144, .T. ) ;
#1093 = FACE_OUTER_BOUND ( 'NONE', #22758, .T. ) ;
#1094 = CARTESIAN_POINT ( 'NONE',  ( 31.81606138205700418, -34.55876147765401640, 70.30501292737011454 ) ) ;
#1095 = DIRECTION ( 'NONE',  ( 0.000000000000000000, 0.7540134720837716742, 0.6568589528324746407 ) ) ;
#1096 = DIRECTION ( 'NONE',  ( 0.000000000000000000, 1.000000000000000000, -2.999999999999999839E-15 ) ) ;
#1097 = EDGE_LOOP ( 'NONE', ( #15045, #20610, #9343, #11397 ) ) ;
#1098 = ORIENTED_EDGE ( 'NONE', *, *, #18616, .F. ) ;
#1099 = AXIS2_PLACEMENT_3D ( 'NONE', #3019, #12833, #12963 ) ;
#1100 = CARTESIAN_POINT ( 'NONE',  ( 43.39709375099405975, 3.108381023609500193, 6.137326095127844994 ) ) ;
#1101 = CARTESIAN_POINT ( 'NONE',  ( 33.31606138205700773, -26.01295748837380373, 65.89261741282676610 ) ) ;
#1102 = AXIS2_PLACEMENT_3D ( 'NONE', #20396, #12433, #2726 ) ;
#1103 = AXIS2_PLACEMENT_3D ( 'NONE', #24593, #16498, #10723 ) ;
#1104 = CARTESIAN_POINT ( 'NONE',  ( 38.26194895904383486, -17.01368208888610312, 70.24448340153875847 ) ) ;
#1105 = ORIENTED_EDGE ( 'NONE', *, *, #4883, .F. ) ;
#1106 = ORIENTED_EDGE ( 'NONE', *, *, #17612, .T. ) ;
#1107 = DIRECTION ( 'NONE',  ( -1.000000000000000000, 5.204170427930415223E-30, 1.734723475976805122E-15 ) ) ;
#1108 = ORIENTED_EDGE ( 'NONE', *, *, #23862, .T. ) ;
#1109 = CARTESIAN_POINT ( 'NONE',  ( 39.95015449827720744, -0.6136820888861040935, 70.79240656858107172 ) ) ;
#1110 = CARTESIAN_POINT ( 'NONE',  ( 36.87297107704149823, -23.90384086642190198, 70.26145752964251301 ) ) ;
#1111 = CARTESIAN_POINT ( 'NONE',  ( 44.06606138205700063, 43.35512946304240245, 82.37823623207322044 ) ) ;
#1112 = CARTESIAN_POINT ( 'NONE',  ( 39.73277004305198545, -8.213682088886105959, 73.23812341099225875 ) ) ;
#1113 = FACE_OUTER_BOUND ( 'NONE', #12163, .T. ) ;
#1114 = DIRECTION ( 'NONE',  ( 0.000000000000000000, -4.116873784215925398E-15, -1.000000000000000000 ) ) ;
#1115 = CARTESIAN_POINT ( 'NONE',  ( 44.81606138205700063, -38.55876147765349771, 84.30501292737325514 ) ) ;
#1116 = CLOSED_SHELL ( 'NONE', ( #23082, #8314, #18083, #5885, #3587, #15410, #23487, #24644, #1224, #14054 ) ) ;
#1117 = ADVANCED_FACE ( 'NONE', ( #22102 ), #16173, .F. ) ;
#1118 = DIRECTION ( 'NONE',  ( 2.011972697750612571E-15, -0.6595716529892353686, 0.7516416929448815898 ) ) ;
#1119 = EDGE_CURVE ( 'NONE', #5642, #11800, #12204, .T. ) ;
#1120 = CIRCLE ( 'NONE', #696, 0.4999999999999982792 ) ;
#1121 = VECTOR ( 'NONE', #18914, 1000.000000000000000 ) ;
#1122 = CARTESIAN_POINT ( 'NONE',  ( 31.81606138205700418, 36.92314894770294131, 80.37823623207323465 ) ) ;
#1123 = PLANE ( 'NONE',  #20476 ) ;
#1124 = EDGE_CURVE ( 'NONE', #13033, #3938, #8531, .T. ) ;
#1125 = DIRECTION ( 'NONE',  ( 0.000000000000000000, 0.000000000000000000, -1.000000000000000000 ) ) ;
#1126 = ORIENTED_EDGE ( 'NONE', *, *, #20228, .T. ) ;
#1127 = DIRECTION ( 'NONE',  ( 0.000000000000000000, 0.7540134720837716742, 0.6568589528324746407 ) ) ;
#1128 = CARTESIAN_POINT ( 'NONE',  ( 47.84183937708599643, -36.05761098950961241, 70.36375082663613512 ) ) ;
#1129 = ORIENTED_EDGE ( 'NONE', *, *, #18715, .T. ) ;
#1130 = VERTEX_POINT ( 'NONE', #12590 ) ;
#1131 = CARTESIAN_POINT ( 'NONE',  ( 39.64521430340305841, -16.80384086642191832, 73.30173637941818754 ) ) ;
#1132 = ADVANCED_FACE ( 'NONE', ( #20048 ), #8586, .T. ) ;
#1133 = CARTESIAN_POINT ( 'NONE',  ( 37.33957961208646736, -21.81368208888610738, 72.81632618279321889 ) ) ;
#1134 = CARTESIAN_POINT ( 'NONE',  ( 33.81606138205700063, 15.19123852234700323, 70.30501292736995822 ) ) ;
#1135 =( GEOMETRIC_REPRESENTATION_CONTEXT ( 3 ) GLOBAL_UNCERTAINTY_ASSIGNED_CONTEXT ( ( #17985 ) ) GLOBAL_UNIT_ASSIGNED_CONTEXT ( ( #4006, #12008, #23702 ) ) REPRESENTATION_CONTEXT ( 'NONE', 'WORKASPACE' ) );
#1136 = AXIS2_PLACEMENT_3D ( 'NONE', #5636, #11329, #11196 ) ;
#1137 = LINE ( 'NONE', #2653, #13495 ) ;
#1138 = ORIENTED_EDGE ( 'NONE', *, *, #21704, .T. ) ;
#1139 = LINE ( 'NONE', #6954, #7217 ) ;
#1140 = CARTESIAN_POINT ( 'NONE',  ( 17.31606138205699708, 42.46194149498198556, 81.44836866983821722 ) ) ;
#1141 = CARTESIAN_POINT ( 'NONE',  ( 39.73277004305198545, -28.21368208888611306, 73.23812341099225875 ) ) ;
#1142 = VERTEX_POINT ( 'NONE', #22358 ) ;
#1143 = CARTESIAN_POINT ( 'NONE',  ( 30.81606138205700418, -10.60718113818700026, 84.30501292737000085 ) ) ;
#1144 = DIRECTION ( 'NONE',  ( 2.727049986597864201E-15, -0.7516416929448760387, -0.6595716529892418079 ) ) ;
#1145 = CARTESIAN_POINT ( 'NONE',  ( 39.75915168707250302, 1.286317911113898260, 70.26145752964255564 ) ) ;
#1146 = LINE ( 'NONE', #22672, #19035 ) ;
#1147 = VERTEX_POINT ( 'NONE', #202 ) ;
#1148 = CARTESIAN_POINT ( 'NONE',  ( 36.64852494920107517, -19.41368208888610525, 70.89533451361947414 ) ) ;
#1149 = DIRECTION ( 'NONE',  ( 0.000000000000000000, 0.7540134720837716742, 0.6568589528324746407 ) ) ;
#1150 = CARTESIAN_POINT ( 'NONE',  ( 33.31606138205700773, -19.73594837544667513, 24.33996001444790025 ) ) ;
#1151 = CARTESIAN_POINT ( 'NONE',  ( 37.60469502381300799, -20.40384086642191264, 72.26730301774234988 ) ) ;
#1152 = CARTESIAN_POINT ( 'NONE',  ( 39.29254315202756231, -4.813682088886099386, 69.94417936956673998 ) ) ;
#1153 = AXIS2_PLACEMENT_3D ( 'NONE', #1229, #14385, #6785 ) ;
#1154 = EDGE_LOOP ( 'NONE', ( #13545, #20999, #8153, #9864 ) ) ;
#1155 = CARTESIAN_POINT ( 'NONE',  ( 31.81606138205700418, -34.55876147765401640, 70.30501292737011454 ) ) ;
#1156 = VERTEX_POINT ( 'NONE', #2386 ) ;
#1157 = AXIS2_PLACEMENT_3D ( 'NONE', #10550, #22012, #733 ) ;
#1158 = CARTESIAN_POINT ( 'NONE',  ( 40.14115730948191185, -5.103840866421909261, 71.43714994484034264 ) ) ;
#1159 = CARTESIAN_POINT ( 'NONE',  ( 32.81606138205700773, -20.26871824316192061, 44.92082169825412308 ) ) ;
#1160 = ADVANCED_FACE ( 'NONE', ( #8080 ), #18126, .T. ) ;
#1161 = CARTESIAN_POINT ( 'NONE',  ( 39.98359781491296161, -6.413682088886103472, 71.86517103874048473 ) ) ;
#1162 = EDGE_LOOP ( 'NONE', ( #24133, #21843, #12662, #15082 ) ) ;
#1163 = CARTESIAN_POINT ( 'NONE',  ( 39.02088643472237095, -6.913682088886101695, 69.02690120949094421 ) ) ;
#1164 = ORIENTED_EDGE ( 'NONE', *, *, #19083, .T. ) ;
#1165 = CARTESIAN_POINT ( 'NONE',  ( 32.81606138205700773, -3.566646240838321269, 18.16837712155798457 ) ) ;
#1166 = CARTESIAN_POINT ( 'NONE',  ( 39.31564783533279694, -11.30384086642191299, 70.72433947564853440 ) ) ;
#1167 = VECTOR ( 'NONE', #35, 1000.000000000000000 ) ;
#1168 = CARTESIAN_POINT ( 'NONE',  ( 40.31606138205700773, -10.19550266980813014, 14.63954348514304904 ) ) ;
#1169 = ORIENTED_EDGE ( 'NONE', *, *, #18390, .F. ) ;
#1170 = DIRECTION ( 'NONE',  ( 1.180247624328911721E-15, -0.3934158747763039088, 0.9193606199277819524 ) ) ;
#1171 = CARTESIAN_POINT ( 'NONE',  ( 37.31606138205699352, -10.61256217995208395, 37.48782943861662176 ) ) ;
#1172 = CARTESIAN_POINT ( 'NONE',  ( 39.12911128074872380, -17.50384086642191406, 69.06206559358665231 ) ) ;
#1173 = VECTOR ( 'NONE', #6959, 1000.000000000000000 ) ;
#1174 = CARTESIAN_POINT ( 'NONE',  ( 36.32862050049384806, -20.47881959453051692, 75.45202403124359591 ) ) ;
#1175 = AXIS2_PLACEMENT_3D ( 'NONE', #24620, #8563, #4942 ) ;
#1176 = DIRECTION ( 'NONE',  ( -1.000000000000000000, 4.152573584826051666E-20, -5.976021130153593973E-20 ) ) ;
#1177 = CARTESIAN_POINT ( 'NONE',  ( 38.93415946300897446, -20.11368208888610809, 73.09843995877329803 ) ) ;
#1178 = PLANE ( 'NONE',  #7609 ) ;
#1179 = DIRECTION ( 'NONE',  ( 0.000000000000000000, 1.000000000000000000, -2.999999999999999839E-15 ) ) ;
#1180 = EDGE_CURVE ( 'NONE', #7272, #21608, #20308, .T. ) ;
#1181 = CIRCLE ( 'NONE', #15586, 1.500000000000001332 ) ;
#1182 = ORIENTED_EDGE ( 'NONE', *, *, #7364, .T. ) ;
#1183 = DIRECTION ( 'NONE',  ( 0.000000000000000000, 0.5703958094953464064, 0.8213699656732943444 ) ) ;
#1184 = ADVANCED_FACE ( 'NONE', ( #6400 ), #19925, .T. ) ;
#1185 = LINE ( 'NONE', #1315, #3185 ) ;
#1186 = CARTESIAN_POINT ( 'NONE',  ( 38.82593461698264292, -6.703840866421915123, 73.13360434286904876 ) ) ;
#1187 = DIRECTION ( 'NONE',  ( 0.000000000000000000, -1.000000000000000000, 2.999999999999999839E-15 ) ) ;
#1188 = AXIS2_PLACEMENT_3D ( 'NONE', #5142, #18661, #1125 ) ;
#1189 = EDGE_CURVE ( 'NONE', #17007, #11300, #6517, .T. ) ;
#1190 = CARTESIAN_POINT ( 'NONE',  ( 39.98359781491296161, -22.41368208888610525, 71.86517103874047052 ) ) ;
#1191 = LINE ( 'NONE', #21171, #9841 ) ;
#1192 = COLOUR_RGB ( '', 0.31764706, 0.68627451, 0.89019608) ;
#1193 = CARTESIAN_POINT ( 'NONE',  ( 36.80608444377001831, -22.30384086642191477, 72.40698646996135324 ) ) ;
#1194 = CARTESIAN_POINT ( 'NONE',  ( 43.81608638205700146, -3.566646240838321269, 18.16837712155798457 ) ) ;
#1195 = AXIS2_PLACEMENT_3D ( 'NONE', #20880, #3219, #19198 ) ;
#1196 = EDGE_CURVE ( 'NONE', #13325, #17789, #3167, .T. ) ;
#1197 = CARTESIAN_POINT ( 'NONE',  ( 39.75915168707250302, -24.71368208888610241, 70.26145752964249880 ) ) ;
#1198 = ORIENTED_EDGE ( 'NONE', *, *, #14465, .F. ) ;
#1199 = VERTEX_POINT ( 'NONE', #12332 ) ;
#1200 = CARTESIAN_POINT ( 'NONE',  ( 32.81606138205700773, -27.60498114914039647, 57.04949906928990089 ) ) ;
#1201 = DIRECTION ( 'NONE',  ( 1.000000000000000000, 1.734723475976804876E-16, -1.734723475976814737E-16 ) ) ;
#1202 = CARTESIAN_POINT ( 'NONE',  ( 39.41296390513587511, -0.4136820888861019174, 71.67976084211552745 ) ) ;
#1203 = VECTOR ( 'NONE', #13238, 999.9999999999998863 ) ;
#1204 = ORIENTED_EDGE ( 'NONE', *, *, #24429, .F. ) ;
#1205 = VERTEX_POINT ( 'NONE', #14003 ) ;
#1206 = FACE_OUTER_BOUND ( 'NONE', #18017, .T. ) ;
#1207 = CARTESIAN_POINT ( 'NONE',  ( 43.24580177837434292, 3.721690752961224202, 6.335617458560805382 ) ) ;
#1208 = ORIENTED_EDGE ( 'NONE', *, *, #18160, .F. ) ;
#1209 = CARTESIAN_POINT ( 'NONE',  ( 36.64852494920107517, -2.203840866421912015, 71.86517103874049894 ) ) ;
#1210 = VECTOR ( 'NONE', #15431, 1000.000000000000000 ) ;
#1211 = VECTOR ( 'NONE', #15036, 1000.000000000000000 ) ;
#1212 = LINE ( 'NONE', #10894, #2646 ) ;
#1213 = DIRECTION ( 'NONE',  ( -1.000000000000000078E-15, 0.9439899321577400748, 0.3299742535180970049 ) ) ;
#1214 = ORIENTED_EDGE ( 'NONE', *, *, #12103, .F. ) ;
#1215 = EDGE_CURVE ( 'NONE', #21718, #13011, #24273, .T. ) ;
#1216 = EDGE_LOOP ( 'NONE', ( #10411, #24861, #10562, #15495, #17319, #20995, #18206, #9644 ) ) ;
#1217 = VECTOR ( 'NONE', #3864, 1000.000000000000000 ) ;
#1218 = CARTESIAN_POINT ( 'NONE',  ( 33.40064408022072939, 42.57231754924293909, 79.37823623207320622 ) ) ;
#1219 = EDGE_CURVE ( 'NONE', #1205, #10773, #20042, .T. ) ;
#1220 = CARTESIAN_POINT ( 'NONE',  ( 37.80618814713140097, -3.913682088886108357, 73.13360434286904876 ) ) ;
#1221 = EDGE_CURVE ( 'NONE', #7327, #16296, #2262, .T. ) ;
#1222 = PRESENTATION_STYLE_ASSIGNMENT (( #4371 ) ) ;
#1223 = PLANE ( 'NONE',  #24789 ) ;
#1224 = ADVANCED_FACE ( 'NONE', ( #14501 ), #8936, .T. ) ;
#1225 = AXIS2_PLACEMENT_3D ( 'NONE', #6385, #8318, #16034 ) ;
#1226 = EDGE_CURVE ( 'NONE', #15804, #2469, #13867, .T. ) ;
#1227 = ORIENTED_EDGE ( 'NONE', *, *, #6032, .F. ) ;
#1228 = VECTOR ( 'NONE', #9593, 1000.000000000000000 ) ;
#1229 = CARTESIAN_POINT ( 'NONE',  ( 32.81606138205700773, 36.92314894770294131, 81.37823623207324886 ) ) ;
#1230 = LINE ( 'NONE', #8371, #20694 ) ;
#1231 = AXIS2_PLACEMENT_3D ( 'NONE', #23636, #18106, #21584 ) ;
#1232 = DIRECTION ( 'NONE',  ( 1.000000000000000000, 2.999999999999999839E-15, 0.000000000000000000 ) ) ;
#1233 = LINE ( 'NONE', #1359, #7332 ) ;
#1234 = FILL_AREA_STYLE_COLOUR ( '', #7978 ) ;
#1235 = EDGE_CURVE ( 'NONE', #1331, #1701, #323, .T. ) ;
#1236 = FACE_OUTER_BOUND ( 'NONE', #11990, .T. ) ;
#1237 = ORIENTED_EDGE ( 'NONE', *, *, #24724, .T. ) ;
#1238 = ORIENTED_EDGE ( 'NONE', *, *, #21451, .T. ) ;
#1239 = EDGE_CURVE ( 'NONE', #16406, #17655, #12232, .T. ) ;
#1240 = DIRECTION ( 'NONE',  ( 1.000000000000000000, -0.000000000000000000, 0.000000000000000000 ) ) ;
#1241 = ADVANCED_BREP_SHAPE_REPRESENTATION ( '', ( #17413, #2000 ), #7588 ) ;
#1242 = DIRECTION ( 'NONE',  ( 0.000000000000000000, 1.000000000000000000, 0.000000000000000000 ) ) ;
#1243 = CARTESIAN_POINT ( 'NONE',  ( 39.41296390513587511, -18.41368208888610170, 71.67976084211551324 ) ) ;
#1244 = VERTEX_POINT ( 'NONE', #17079 ) ;
#1245 = ORIENTED_EDGE ( 'NONE', *, *, #19719, .F. ) ;
#1246 = LINE ( 'NONE', #9127, #504 ) ;
#1247 = CARTESIAN_POINT ( 'NONE',  ( 39.95015449827720744, -2.613682088886105870, 70.79240656858107172 ) ) ;
#1248 = CARTESIAN_POINT ( 'NONE',  ( 39.75915168707251723, -20.90384086642190553, 72.49904802271738902 ) ) ;
#1249 = AXIS2_PLACEMENT_3D ( 'NONE', #3363, #10974, #11240 ) ;
#1250 = CARTESIAN_POINT ( 'NONE',  ( 38.31606138205700063, 37.69123852234599781, 71.30501292737001506 ) ) ;
#1251 = EDGE_CURVE ( 'NONE', #3863, #5274, #4832, .T. ) ;
#1252 = CARTESIAN_POINT ( 'NONE',  ( 36.98690846071097837, -3.813682088886109156, 73.30173637941818754 ) ) ;
#1253 = VECTOR ( 'NONE', #12245, 1000.000000000000227 ) ;
#1254 = DIRECTION ( 'NONE',  ( 1.000000000000000000, 3.194449454093636853E-15, 9.596449257708899394E-17 ) ) ;
#1255 = EDGE_LOOP ( 'NONE', ( #21618, #11872, #14334, #19616 ) ) ;
#1256 = CARTESIAN_POINT ( 'NONE',  ( 33.31606138205700773, 10.62769494289597993, 68.29765714199933768 ) ) ;
#1257 = CARTESIAN_POINT ( 'NONE',  ( 32.56606138205700773, 43.35512946304240245, 82.37823623207322044 ) ) ;
#1258 = DIRECTION ( 'NONE',  ( 1.327674326049719602E-15, -0.4425581086832399147, 0.8967398287344627850 ) ) ;
#1259 = DIRECTION ( 'NONE',  ( 0.000000000000000000, 1.000000000000000000, -5.551115123125785858E-15 ) ) ;
#1260 = LINE ( 'NONE', #24820, #4453 ) ;
#1261 = PRODUCT_DEFINITION_SHAPE ( 'NONE', 'NONE',  #25499 ) ;
#1262 = CARTESIAN_POINT ( 'NONE',  ( 33.31606138205700773, 6.366250835946937414, 6.636353555660924997 ) ) ;
#1263 = ORIENTED_EDGE ( 'NONE', *, *, #4909, .F. ) ;
#1264 = VECTOR ( 'NONE', #4201, 1000.000000000000000 ) ;
#1265 = CARTESIAN_POINT ( 'NONE',  ( 41.81606138205700063, -14.36460986495925241, 36.24727600202827915 ) ) ;
#1266 = DIRECTION ( 'NONE',  ( -1.327674326049719602E-15, 0.4425581086832399147, -0.8967398287344627850 ) ) ;
#1267 = ORIENTED_EDGE ( 'NONE', *, *, #5167, .T. ) ;
#1268 = ORIENTED_EDGE ( 'NONE', *, *, #6443, .F. ) ;
#1269 = CIRCLE ( 'NONE', #22659, 1.499999999999999778 ) ;
#1270 = CARTESIAN_POINT ( 'NONE',  ( 35.86008812008917346, -18.10384086642191548, 71.32335560751961623 ) ) ;
#1271 = CARTESIAN_POINT ( 'NONE',  ( 42.65336712727322777, 3.163553052512885877, 6.379934517999310550 ) ) ;
#1272 = CARTESIAN_POINT ( 'NONE',  ( 39.98359781491296161, -18.41368208888610880, 71.86517103874047052 ) ) ;
#1273 = DIRECTION ( 'NONE',  ( 0.000000000000000000, 0.8191520442889929088, 0.5735764363510444941 ) ) ;
#1274 = ADVANCED_FACE ( 'NONE', ( #3147 ), #15131, .T. ) ;
#1275 = ADVANCED_FACE ( 'NONE', ( #8845 ), #16686, .F. ) ;
#1276 = ORIENTED_EDGE ( 'NONE', *, *, #23502, .F. ) ;
#1277 = FACE_OUTER_BOUND ( 'NONE', #6390, .T. ) ;
#1278 = DIRECTION ( 'NONE',  ( -2.602085213965212219E-15, 0.8967398287344632291, 0.4425581086832389155 ) ) ;
#1279 = CARTESIAN_POINT ( 'NONE',  ( 37.61123632939164452, 0.2961591335780902612, 69.02690120949095842 ) ) ;
#1280 = ORIENTED_EDGE ( 'NONE', *, *, #19495, .T. ) ;
#1281 = FACE_OUTER_BOUND ( 'NONE', #17840, .T. ) ;
#1282 = CARTESIAN_POINT ( 'NONE',  ( 39.82603832034400426, -2.313682088886107380, 72.40698646996135324 ) ) ;
#1283 = CARTESIAN_POINT ( 'NONE',  ( 43.31606138205700063, -5.204193249396356968, 72.80501292736992980 ) ) ;
#1284 = CARTESIAN_POINT ( 'NONE',  ( 36.87297107704153376, -15.71368208888610596, 72.49904802271740323 ) ) ;
#1285 = AXIS2_PLACEMENT_3D ( 'NONE', #5753, #3813, #23012 ) ;
#1286 = CARTESIAN_POINT ( 'NONE',  ( 38.83707137437546919, -22.15989686853476925, 75.80517981147842477 ) ) ;
#1287 = CYLINDRICAL_SURFACE ( 'NONE', #11276, 3.000000000000000000 ) ;
#1288 = CARTESIAN_POINT ( 'NONE',  ( 37.12184278917507640, -20.10384086642191193, 71.32335560751961623 ) ) ;
#1289 = CARTESIAN_POINT ( 'NONE',  ( 39.82603832034400426, -6.313682088886107380, 72.40698646996135324 ) ) ;
#1290 = ORIENTED_EDGE ( 'NONE', *, *, #23271, .T. ) ;
#1291 = CARTESIAN_POINT ( 'NONE',  ( 46.91606138205697363, -29.47337283097070681, 44.07055847651734837 ) ) ;
#1292 = ORIENTED_EDGE ( 'NONE', *, *, #10707, .F. ) ;
#1293 = CARTESIAN_POINT ( 'NONE',  ( 36.87297107704149823, -7.903840866421908196, 70.26145752964255564 ) ) ;
#1294 = CARTESIAN_POINT ( 'NONE',  ( 33.31606138205700773, -16.48551471403133206, 77.11349248448009064 ) ) ;
#1295 = CARTESIAN_POINT ( 'NONE',  ( 39.31564783533280405, -28.31368208888610383, 72.03616607671136762 ) ) ;
#1296 = VERTEX_POINT ( 'NONE', #10772 ) ;
#1297 = CARTESIAN_POINT ( 'NONE',  ( 37.61123632939165873, -9.913682088886107024, 73.73360434286902887 ) ) ;
#1298 = ORIENTED_EDGE ( 'NONE', *, *, #21210, .T. ) ;
#1299 = CARTESIAN_POINT ( 'NONE',  ( 28.84183937708599998, -33.05991196579839198, 70.24627502810386659 ) ) ;
#1300 = EDGE_CURVE ( 'NONE', #23758, #7648, #9233, .T. ) ;
#1301 = CARTESIAN_POINT ( 'NONE',  ( 39.51027997493896748, -9.103840866421911926, 71.43714994484034264 ) ) ;
#1302 = EDGE_CURVE ( 'NONE', #5803, #15873, #5351, .T. ) ;
#1303 = ORIENTED_EDGE ( 'NONE', *, *, #4139, .F. ) ;
#1304 = ORIENTED_EDGE ( 'NONE', *, *, #10169, .T. ) ;
#1305 = CARTESIAN_POINT ( 'NONE',  ( 43.31606138205700063, -4.357181138186123626, 83.30501292736992980 ) ) ;
#1306 = DIRECTION ( 'NONE',  ( -1.734723475976804876E-16, -3.469446951953610245E-15, -1.000000000000000000 ) ) ;
#1307 = CARTESIAN_POINT ( 'NONE',  ( 36.89935272106205133, -14.40384086642191974, 73.23812341099225875 ) ) ;
#1308 = PLANE ( 'NONE',  #18193 ) ;
#1309 =( LENGTH_UNIT ( ) NAMED_UNIT ( * ) SI_UNIT ( .MILLI., .METRE. ) );
#1310 = CARTESIAN_POINT ( 'NONE',  ( 37.33957961208646736, -21.81368208888610738, 72.81632618279321889 ) ) ;
#1311 = CARTESIAN_POINT ( 'NONE',  ( 33.31606138205700773, -21.39087554181784512, 28.82307548518892304 ) ) ;
#1312 = DIRECTION ( 'NONE',  ( 0.000000000000000000, 1.000000000000000000, -2.999999999999999839E-15 ) ) ;
#1313 = ORIENTED_EDGE ( 'NONE', *, *, #19104, .T. ) ;
#1314 = DIRECTION ( 'NONE',  ( 1.189524669241238159E-14, 1.000000000000000000, -3.965082230804126670E-15 ) ) ;
#1315 = CARTESIAN_POINT ( 'NONE',  ( 40.31606138205700773, -14.15704008206720843, 14.73030834591676808 ) ) ;
#1316 = EDGE_CURVE ( 'NONE', #2214, #22818, #6046, .T. ) ;
#1317 = AXIS2_PLACEMENT_3D ( 'NONE', #11954, #4341, #2385 ) ;
#1318 = CARTESIAN_POINT ( 'NONE',  ( 37.33957961208645315, -7.803840866421909439, 69.94417936956673998 ) ) ;
#1319 = SHAPE_DEFINITION_REPRESENTATION ( #23060, #7525 ) ;
#1320 = AXIS2_PLACEMENT_3D ( 'NONE', #1883, #23395, #7445 ) ;
#1321 = DIRECTION ( 'NONE',  ( 0.000000000000000000, 0.5706330172266920187, -0.8212051873014210024 ) ) ;
#1322 = CARTESIAN_POINT ( 'NONE',  ( 36.64852494920107517, -27.41368208888610525, 70.89533451361945993 ) ) ;
#1323 = DIRECTION ( 'NONE',  ( 0.000000000000000000, 0.000000000000000000, 1.000000000000000000 ) ) ;
#1324 = AXIS2_PLACEMENT_3D ( 'NONE', #12607, #16567, #16067 ) ;
#1325 = CARTESIAN_POINT ( 'NONE',  ( 37.80618814713138676, -21.70384086642190979, 69.62690120949091011 ) ) ;
#1326 = CARTESIAN_POINT ( 'NONE',  ( 37.67019652925851148, -5.306827745754475245, 83.30968309601763622 ) ) ;
#1327 = CIRCLE ( 'NONE', #20258, 1.750000000000001554 ) ;
#1328 = CARTESIAN_POINT ( 'NONE',  ( 39.95015449827720744, -18.61368208888610454, 70.79240656858105751 ) ) ;
#1329 = ORIENTED_EDGE ( 'NONE', *, *, #12339, .T. ) ;
#1330 = CARTESIAN_POINT ( 'NONE',  ( 39.02088643472237095, -26.91368208888610170, 69.02690120949091579 ) ) ;
#1331 = VERTEX_POINT ( 'NONE', #14748 ) ;
#1332 = CARTESIAN_POINT ( 'NONE',  ( 33.23377616717382921, 3.110315666471061391, 6.136481299340784012 ) ) ;
#1333 = DIRECTION ( 'NONE',  ( -1.000000000000000000, 5.204170427930415223E-30, 1.734723475976805122E-15 ) ) ;
#1334 = CARTESIAN_POINT ( 'NONE',  ( 39.37952058850012804, 1.386317911113897683, 70.97781676520604321 ) ) ;
#1335 = ORIENTED_EDGE ( 'NONE', *, *, #4372, .F. ) ;
#1336 = ORIENTED_EDGE ( 'NONE', *, *, #19490, .T. ) ;
#1337 = CARTESIAN_POINT ( 'NONE',  ( 32.81606138205700773, 2.191238522347013440, 73.80501292737000085 ) ) ;
#1338 = CARTESIAN_POINT ( 'NONE',  ( 30.81606138205700418, 1.142818861812999742, 84.30501292737000085 ) ) ;
#1339 = EDGE_LOOP ( 'NONE', ( #19131, #24920, #3494, #3969 ) ) ;
#1340 = CYLINDRICAL_SURFACE ( 'NONE', #15171, 9.500000000000000000 ) ;
#1341 = CARTESIAN_POINT ( 'NONE',  ( 39.38009889167648936, -7.403840866421908196, 70.00779233799264034 ) ) ;
#1342 = VECTOR ( 'NONE', #18259, 1000.000000000000000 ) ;
#1343 = PLANE ( 'NONE',  #12552 ) ;
#1344 = AXIS2_PLACEMENT_3D ( 'NONE', #22886, #23011, #20710 ) ;
#1345 = LINE ( 'NONE', #22733, #4452 ) ;
#1346 = ORIENTED_EDGE ( 'NONE', *, *, #18533, .T. ) ;
#1347 = ORIENTED_EDGE ( 'NONE', *, *, #10592, .F. ) ;
#1348 = CARTESIAN_POINT ( 'NONE',  ( 32.81606138205700773, -1.677874310045055051, 19.48083306117937852 ) ) ;
#1349 = CARTESIAN_POINT ( 'NONE',  ( 39.75915168707250302, -0.7136820888860999634, 70.26145752964255564 ) ) ;
#1350 = VECTOR ( 'NONE', #7285, 1000.000000000000000 ) ;
#1351 = ADVANCED_FACE ( 'NONE', ( #6774 ), #24897, .T. ) ;
#1352 = DIRECTION ( 'NONE',  ( -1.000000000000000000, 1.115179377413661005E-30, 3.717264591378870232E-16 ) ) ;
#1353 = CARTESIAN_POINT ( 'NONE',  ( 30.81606138205700418, 40.39281886181299797, 82.55501292736983032 ) ) ;
#1354 = ORIENTED_EDGE ( 'NONE', *, *, #20276, .F. ) ;
#1355 = CARTESIAN_POINT ( 'NONE',  ( 29.81606138205696155, -0.7562224151693598406, -1.633662118351544734 ) ) ;
#1356 = VECTOR ( 'NONE', #1201, 1000.000000000000000 ) ;
#1357 = AXIS2_PLACEMENT_3D ( 'NONE', #18223, #4569, #15775 ) ;
#1358 = LINE ( 'NONE', #13469, #4116 ) ;
#1359 = CARTESIAN_POINT ( 'NONE',  ( 38.31606138205700063, -29.30876147765400574, 73.55501292737010033 ) ) ;
#1360 = ORIENTED_EDGE ( 'NONE', *, *, #12429, .F. ) ;
#1361 = VECTOR ( 'NONE', #5593, 1000.000000000000000 ) ;
#1362 = FACE_OUTER_BOUND ( 'NONE', #24504, .T. ) ;
#1363 = VERTEX_POINT ( 'NONE', #4965 ) ;
#1364 = ORIENTED_EDGE ( 'NONE', *, *, #18759, .T. ) ;
#1365 = CARTESIAN_POINT ( 'NONE',  ( 32.81606138205700773, 2.191238522347013440, 73.80501292737000085 ) ) ;
#1366 = DIRECTION ( 'NONE',  ( 1.225631768639319301E-15, -0.4425581086832399147, 0.8967398287344627850 ) ) ;
#1367 = ADVANCED_FACE ( 'NONE', ( #22480 ), #8716, .F. ) ;
#1368 = EDGE_CURVE ( 'NONE', #9987, #15268, #10993, .T. ) ;
#1369 = CARTESIAN_POINT ( 'NONE',  ( 37.12184278917507640, -15.51368208888610312, 71.43714994484034264 ) ) ;
#1370 = ORIENTED_EDGE ( 'NONE', *, *, #10698, .F. ) ;
#1371 = AXIS2_PLACEMENT_3D ( 'NONE', #16139, #21574, #22069 ) ;
#1372 = ORIENTED_EDGE ( 'NONE', *, *, #7692, .T. ) ;
#1373 = CARTESIAN_POINT ( 'NONE',  ( 39.48763425731081611, -22.27515649656511343, 29.48506754039016542 ) ) ;
#1374 = LINE ( 'NONE', #5377, #11185 ) ;
#1375 = CARTESIAN_POINT ( 'NONE',  ( 36.49096545463212493, -24.10384086642190482, 71.32335560751960202 ) ) ;
#1376 = EDGE_CURVE ( 'NONE', #15787, #6943, #9101, .T. ) ;
#1377 = ADVANCED_FACE ( 'NONE', ( #1082 ), #8967, .T. ) ;
#1378 = EDGE_CURVE ( 'NONE', #559, #12298, #7156, .T. ) ;
#1379 = DIRECTION ( 'NONE',  ( 1.000000000000000000, 1.289685230616452080E-30, -8.343550184191211817E-45 ) ) ;
#1380 = CARTESIAN_POINT ( 'NONE',  ( 38.37017380507020192, -4.013682088886107557, 73.71602215082116061 ) ) ;
#1381 = VECTOR ( 'NONE', #22924, 1000.000000000000000 ) ;
#1382 = ORIENTED_EDGE ( 'NONE', *, *, #10274, .T. ) ;
#1383 = FACE_OUTER_BOUND ( 'NONE', #17604, .T. ) ;
#1384 = VECTOR ( 'NONE', #12923, 1000.000000000000000 ) ;
#1385 = EDGE_CURVE ( 'NONE', #23504, #12932, #9806, .T. ) ;
#1386 = DIRECTION ( 'NONE',  ( 9.925461516413221718E-16, -0.8967398287344632291, -0.4425581086832394151 ) ) ;
#1387 = EDGE_CURVE ( 'NONE', #21411, #6994, #5221, .T. ) ;
#1388 = DIRECTION ( 'NONE',  ( 0.000000000000000000, 1.000000000000000000, -3.469446951953614189E-15 ) ) ;
#1389 = CARTESIAN_POINT ( 'NONE',  ( 44.81606138205700063, -24.55876147765401285, 70.30501292737008612 ) ) ;
#1390 = CIRCLE ( 'NONE', #150, 1.750000000000001554 ) ;
#1391 = CYLINDRICAL_SURFACE ( 'NONE', #18031, 10.00000000000000000 ) ;
#1392 = CARTESIAN_POINT ( 'NONE',  ( 43.31606138205700063, 6.355893005198818280, 6.643287643123708008 ) ) ;
#1393 = ORIENTED_EDGE ( 'NONE', *, *, #3030, .T. ) ;
#1394 = CARTESIAN_POINT ( 'NONE',  ( 41.31606138205687273, 42.19123852234595518, 61.80501292736988006 ) ) ;
#1395 = EDGE_CURVE ( 'NONE', #20256, #6631, #1345, .T. ) ;
#1396 = PLANE ( 'NONE',  #6605 ) ;
#1397 = EDGE_LOOP ( 'NONE', ( #14568, #17357, #12669, #9728 ) ) ;
#1398 = ORIENTED_EDGE ( 'NONE', *, *, #6590, .T. ) ;
#1399 = CIRCLE ( 'NONE', #21957, 9.500000000000000000 ) ;
#1400 = CARTESIAN_POINT ( 'NONE',  ( 36.98690846071097127, -11.80384086642191477, 69.45876917294175712 ) ) ;
#1401 = AXIS2_PLACEMENT_3D ( 'NONE', #3846, #7337, #9406 ) ;
#1402 = LINE ( 'NONE', #7459, #2527 ) ;
#1403 = CARTESIAN_POINT ( 'NONE',  ( 38.82593461698262871, -18.91368208888609459, 69.62690120949091011 ) ) ;
#1404 = ORIENTED_EDGE ( 'NONE', *, *, #22708, .F. ) ;
#1405 = CARTESIAN_POINT ( 'NONE',  ( 33.56606138205700773, 41.44123852234599070, 73.55501292736987295 ) ) ;
#1406 = CARTESIAN_POINT ( 'NONE',  ( 43.81606138205700063, 35.95440708241085304, 61.30501292736990138 ) ) ;
#1407 = CARTESIAN_POINT ( 'NONE',  ( 40.33642880535524000, -22.31368208888610738, 72.77780686321126780 ) ) ;
#1408 = ORIENTED_EDGE ( 'NONE', *, *, #1499, .T. ) ;
#1409 = PLANE ( 'NONE',  #22165 ) ;
#1410 = AXIS2_PLACEMENT_3D ( 'NONE', #18726, #1059, #930 ) ;
#1411 = DIRECTION ( 'NONE',  ( -1.000000000000000000, -3.091505625455828697E-15, -4.515976121274772923E-17 ) ) ;
#1412 = LINE ( 'NONE', #8779, #21644 ) ;
#1413 = ADVANCED_FACE ( 'NONE', ( #13587 ), #23234, .T. ) ;
#1414 = CARTESIAN_POINT ( 'NONE',  ( 33.31606138205700773, -18.80550481115971806, 25.27912300651437150 ) ) ;
#1415 = AXIS2_PLACEMENT_3D ( 'NONE', #23739, #15501, #6104 ) ;
#1416 = CARTESIAN_POINT ( 'NONE',  ( 33.40064408022072939, 41.43850569188389699, 79.87823623207322044 ) ) ;
#1417 = CARTESIAN_POINT ( 'NONE',  ( 37.38336156205273397, -21.90384086642191619, 70.63227792289247020 ) ) ;
#1418 = CARTESIAN_POINT ( 'NONE',  ( 37.80618814713140097, -7.913682088886107913, 73.13360434286904876 ) ) ;
#1419 = ORIENTED_EDGE ( 'NONE', *, *, #5165, .F. ) ;
#1420 = CARTESIAN_POINT ( 'NONE',  ( 38.31606138205700063, 39.69123852234599070, 73.55501292736988717 ) ) ;
#1421 = EDGE_CURVE ( 'NONE', #5245, #8986, #7540, .T. ) ;
#1422 = CARTESIAN_POINT ( 'NONE',  ( 39.48763425731081611, -22.27515649656511343, 29.48506754039016897 ) ) ;
#1423 = EDGE_LOOP ( 'NONE', ( #13555, #11688, #6031, #1794, #7597, #21299, #9719 ) ) ;
#1424 = VERTEX_POINT ( 'NONE', #15383 ) ;
#1425 = CARTESIAN_POINT ( 'NONE',  ( 39.12911128074872380, -29.50384086642191050, 69.06206559358663810 ) ) ;
#1426 = CARTESIAN_POINT ( 'NONE',  ( 43.31606138205700063, 7.535758204303438568, 66.26723409915207696 ) ) ;
#1427 = CARTESIAN_POINT ( 'NONE',  ( 39.82603832034400426, -0.3136820888861094336, 72.40698646996135324 ) ) ;
#1428 = CARTESIAN_POINT ( 'NONE',  ( 39.73277004305198545, -6.213682088886108623, 73.23812341099225875 ) ) ;
#1429 = ORIENTED_EDGE ( 'NONE', *, *, #14272, .T. ) ;
#1430 = DIRECTION ( 'NONE',  ( 0.000000000000000000, -2.999999999999999839E-15, -1.000000000000000000 ) ) ;
#1431 = VECTOR ( 'NONE', #1046, 1000.000000000000000 ) ;
#1432 = CARTESIAN_POINT ( 'NONE',  ( 38.63098279924290068, -4.703840866421909794, 72.53360434286905445 ) ) ;
#1433 = DIRECTION ( 'NONE',  ( -1.000000000000000000, 0.000000000000000000, 0.000000000000000000 ) ) ;
#1434 = EDGE_LOOP ( 'NONE', ( #2248, #19526, #19970, #6158 ) ) ;
#1435 = LINE ( 'NONE', #16906, #1000 ) ;
#1436 = DIRECTION ( 'NONE',  ( 2.792262043613788535E-15, -0.8967398287344627850, -0.4425581086832399147 ) ) ;
#1437 = CARTESIAN_POINT ( 'NONE',  ( 38.37017380507018771, -7.603840866421910150, 69.04448340153881247 ) ) ;
#1438 = CARTESIAN_POINT ( 'NONE',  ( 37.66883992158368955, -22.11817844025888036, 75.30541813598723877 ) ) ;
#1439 =( NAMED_UNIT ( * ) SI_UNIT ( $, .STERADIAN. ) SOLID_ANGLE_UNIT ( ) );
#1440 = CARTESIAN_POINT ( 'NONE',  ( 36.64852494920107517, -23.41368208888610525, 70.89533451361945993 ) ) ;
#1441 = DIRECTION ( 'NONE',  ( 3.717264591378870232E-16, 2.999999999999999839E-15, 1.000000000000000000 ) ) ;
#1442 = DIRECTION ( 'NONE',  ( -1.327674326049719602E-15, 0.4425581086832399147, -0.8967398287344627850 ) ) ;
#1443 = ORIENTED_EDGE ( 'NONE', *, *, #14632, .F. ) ;
#1444 = ORIENTED_EDGE ( 'NONE', *, *, #20014, .F. ) ;
#1445 = LINE ( 'NONE', #15479, #291 ) ;
#1446 = CARTESIAN_POINT ( 'NONE',  ( 36.87297107704151244, -9.903840866421905531, 70.26145752964255564 ) ) ;
#1447 = VECTOR ( 'NONE', #3335, 1000.000000000000114 ) ;
#1448 = APPLICATION_PROTOCOL_DEFINITION ( 'draft international standard', 'automotive_design', 1998, #11795 ) ;
#1449 = DIRECTION ( 'NONE',  ( 0.000000000000000000, 0.8212051873014208914, 0.5706330172266919076 ) ) ;
#1450 = CARTESIAN_POINT ( 'NONE',  ( 39.38009889167650357, -22.21368208888610951, 72.75271321436731853 ) ) ;
#1451 = EDGE_CURVE ( 'NONE', #9965, #13296, #11792, .T. ) ;
#1452 = CARTESIAN_POINT ( 'NONE',  ( 33.56606138205700773, 43.19123852234599070, 73.55501292736987295 ) ) ;
#1453 = ADVANCED_FACE ( 'NONE', ( #19133 ), #17457, .T. ) ;
#1454 = CARTESIAN_POINT ( 'NONE',  ( 39.38009889167648936, -21.40384086642190553, 70.00779233799262613 ) ) ;
#1455 = CARTESIAN_POINT ( 'NONE',  ( 36.31606138205700063, -7.205155154158177311, 83.11773453508298815 ) ) ;
#1456 = CARTESIAN_POINT ( 'NONE',  ( 36.68196826583682935, -15.61368208888610454, 71.96809898377888715 ) ) ;
#1457 = ORIENTED_EDGE ( 'NONE', *, *, #2541, .T. ) ;
#1458 = CARTESIAN_POINT ( 'NONE',  ( 36.11133435605973574, -0.003840866421914862494, 70.60699637195612866 ) ) ;
#1459 = ORIENTED_EDGE ( 'NONE', *, *, #3158, .F. ) ;
#1460 = CARTESIAN_POINT ( 'NONE',  ( 33.31606138205700773, -13.58280000135114030, 20.54174511886706256 ) ) ;
#1461 = LINE ( 'NONE', #5711, #20288 ) ;
#1462 = CARTESIAN_POINT ( 'NONE',  ( 39.51027997493896748, -25.10384086642191193, 71.43714994484031422 ) ) ;
#1463 = ORIENTED_EDGE ( 'NONE', *, *, #7053, .F. ) ;
#1464 = ORIENTED_EDGE ( 'NONE', *, *, #574, .T. ) ;
#1465 = DIRECTION ( 'NONE',  ( 1.000000000000000000, 0.000000000000000000, 0.000000000000000000 ) ) ;
#1466 = ADVANCED_FACE ( 'NONE', ( #21311 ), #19623, .F. ) ;
#1467 = CARTESIAN_POINT ( 'NONE',  ( 43.70349364522802205, 3.546438648963166962, 6.213839566231161626 ) ) ;
#1468 = ORIENTED_EDGE ( 'NONE', *, *, #8169, .T. ) ;
#1469 = PLANE ( 'NONE',  #4053 ) ;
#1470 = CARTESIAN_POINT ( 'NONE',  ( 36.87297107704149823, -1.903840866421906419, 70.26145752964255564 ) ) ;
#1471 = FACE_OUTER_BOUND ( 'NONE', #24405, .T. ) ;
#1472 = CARTESIAN_POINT ( 'NONE',  ( 32.81606138205700773, -21.50052602411404834, 44.06487217241408416 ) ) ;
#1473 = ORIENTED_EDGE ( 'NONE', *, *, #15238, .T. ) ;
#1474 = DIRECTION ( 'NONE',  ( 0.000000000000000000, 0.000000000000000000, -1.000000000000000000 ) ) ;
#1475 = CARTESIAN_POINT ( 'NONE',  ( 38.26194895904383486, -3.013682088886100008, 69.64448340153879258 ) ) ;
#1476 = CARTESIAN_POINT ( 'NONE',  ( 38.37017380507018771, -27.60384086642191193, 69.64448340153876416 ) ) ;
#1477 = CARTESIAN_POINT ( 'NONE',  ( 43.81606138205700063, -27.11289203277224402, 56.96090842897168471 ) ) ;
#1478 = EDGE_LOOP ( 'NONE', ( #2621, #21518, #17245, #2091 ) ) ;
#1479 = CARTESIAN_POINT ( 'NONE',  ( 33.31606138205700773, 7.282926244446933595, 65.60596383066929604 ) ) ;
#1480 = CARTESIAN_POINT ( 'NONE',  ( 43.79080625344859357, -32.95845724189726411, 59.23979596822106686 ) ) ;
#1481 = CARTESIAN_POINT ( 'NONE',  ( 37.21915885897815457, -15.41368208888610347, 71.08074471024443142 ) ) ;
#1482 = ORIENTED_EDGE ( 'NONE', *, *, #15615, .T. ) ;
#1483 = CARTESIAN_POINT ( 'NONE',  ( 33.56606138205700773, 41.44123852234595518, 61.30501292736988006 ) ) ;
#1484 = ORIENTED_EDGE ( 'NONE', *, *, #21527, .F. ) ;
#1485 = ORIENTED_EDGE ( 'NONE', *, *, #2006, .T. ) ;
#1486 = DIRECTION ( 'NONE',  ( 7.071067811865491110E-16, -0.9008287146801832179, 0.4341746501209495790 ) ) ;
#1487 = DIRECTION ( 'NONE',  ( 0.000000000000000000, 1.000000000000000000, -2.775557561562891351E-15 ) ) ;
#1488 = CARTESIAN_POINT ( 'NONE',  ( 37.25260217561390874, -11.61368208888610098, 71.78268878715392987 ) ) ;
#1489 = EDGE_LOOP ( 'NONE', ( #16805, #24401, #621, #24675, #16930 ) ) ;
#1490 = EDGE_LOOP ( 'NONE', ( #25234, #19392, #19945, #9121 ) ) ;
#1491 = ADVANCED_FACE ( 'NONE', ( #15640 ), #17326, .F. ) ;
#1492 = CARTESIAN_POINT ( 'NONE',  ( 42.81606138205700063, 16.19123852234703520, 80.30501292736995822 ) ) ;
#1493 = DIRECTION ( 'NONE',  ( 1.000000000000000000, 0.000000000000000000, 0.000000000000000000 ) ) ;
#1494 = CARTESIAN_POINT ( 'NONE',  ( 37.25202387243754032, -22.40384086642191619, 72.75271321436731853 ) ) ;
#1495 = CARTESIAN_POINT ( 'NONE',  ( 42.56606138205700063, 3.151453266960317023, 6.397347472316774031 ) ) ;
#1496 = PLANE ( 'NONE',  #16992 ) ;
#1497 = CARTESIAN_POINT ( 'NONE',  ( 33.31606138205700773, -20.93319939328399926, 43.78741072286599945 ) ) ;
#1498 = CARTESIAN_POINT ( 'NONE',  ( 32.81606138205700773, 46.92314894770293421, 79.37823623207319201 ) ) ;
#1499 = EDGE_CURVE ( 'NONE', #17110, #23130, #1965, .T. ) ;
#1500 = EDGE_CURVE ( 'NONE', #14863, #19510, #21440, .T. ) ;
#1501 = CARTESIAN_POINT ( 'NONE',  ( 39.91050633825327054, -5.952338289763780210, 82.77753289558458505 ) ) ;
#1502 = DIRECTION ( 'NONE',  ( -1.000000000000000000, 0.000000000000000000, 0.000000000000000000 ) ) ;
#1503 = CARTESIAN_POINT ( 'NONE',  ( 37.31606138205700063, 43.19123852234599070, 73.55501292736987295 ) ) ;
#1504 = ADVANCED_FACE ( 'NONE', ( #3782 ), #23485, .F. ) ;
#1505 = AXIS2_PLACEMENT_3D ( 'NONE', #21822, #6491, #10492 ) ;
#1506 = AXIS2_PLACEMENT_3D ( 'NONE', #4542, #12406, #10968 ) ;
#1507 = ORIENTED_EDGE ( 'NONE', *, *, #799, .T. ) ;
#1508 = CARTESIAN_POINT ( 'NONE',  ( 45.81606138205700063, 46.92314894770294131, 81.17823623207320338 ) ) ;
#1509 = CARTESIAN_POINT ( 'NONE',  ( 43.38751061443460344, 3.099069811988895751, 6.135932541694130826 ) ) ;
#1510 = VERTEX_POINT ( 'NONE', #1472 ) ;
#1511 = ORIENTED_EDGE ( 'NONE', *, *, #22943, .F. ) ;
#1512 = CARTESIAN_POINT ( 'NONE',  ( 36.98690846071097127, -13.80384086642191122, 69.45876917294175712 ) ) ;
#1513 = EDGE_CURVE ( 'NONE', #4468, #8243, #13715, .T. ) ;
#1514 = CARTESIAN_POINT ( 'NONE',  ( 29.81606138205705037, -30.46100403034036219, 72.05704881431053366 ) ) ;
#1515 = CARTESIAN_POINT ( 'NONE',  ( 39.82603832034400426, -12.31368208888610560, 72.40698646996133903 ) ) ;
#1516 = ORIENTED_EDGE ( 'NONE', *, *, #15444, .F. ) ;
#1517 = CARTESIAN_POINT ( 'NONE',  ( 36.31606138205700773, -19.13113579875042092, 24.60350147050422720 ) ) ;
#1518 = CARTESIAN_POINT ( 'NONE',  ( 33.31606138205700773, 7.535758204303438568, 66.26723409915207696 ) ) ;
#1519 = CARTESIAN_POINT ( 'NONE',  ( 37.50301148336529167, -23.11368208888610454, 69.06206559358663810 ) ) ;
#1520 = VERTEX_POINT ( 'NONE', #21571 ) ;
#1521 = FACE_BOUND ( 'NONE', #18539, .T. ) ;
#1522 = AXIS2_PLACEMENT_3D ( 'NONE', #25307, #23255, #13610 ) ;
#1523 = CARTESIAN_POINT ( 'NONE',  ( 33.71979045277213061, 3.032422752665409060, 6.234282092415138976 ) ) ;
#1524 = CARTESIAN_POINT ( 'NONE',  ( 34.81606138205700773, -20.93319939328399926, 43.78741072286599945 ) ) ;
#1525 = ADVANCED_FACE ( 'NONE', ( #3920 ), #7918, .F. ) ;
#1526 = CARTESIAN_POINT ( 'NONE',  ( 43.79080625344859357, -32.95845724189726411, 59.23979596822106686 ) ) ;
#1527 = CARTESIAN_POINT ( 'NONE',  ( 31.91606138205697363, -4.349482454670880571, -5.142398479549302515 ) ) ;
#1528 = EDGE_CURVE ( 'NONE', #14570, #22793, #25149, .T. ) ;
#1529 = CARTESIAN_POINT ( 'NONE',  ( 38.93987200065210175, -10.80384086642191299, 72.33091598616827866 ) ) ;
#1530 = CARTESIAN_POINT ( 'NONE',  ( 39.38009889167650357, -0.2136820888861065693, 72.75271321436733274 ) ) ;
#1531 = EDGE_CURVE ( 'NONE', #4589, #5235, #15503, .T. ) ;
#1532 = ORIENTED_EDGE ( 'NONE', *, *, #20926, .F. ) ;
#1533 = LINE ( 'NONE', #24854, #22186 ) ;
#1534 = DIRECTION ( 'NONE',  ( -1.000000000000000000, -1.000000000000000078E-15, 0.000000000000000000 ) ) ;
#1535 = EDGE_LOOP ( 'NONE', ( #11960, #24521, #19321, #10094 ) ) ;
#1536 = CIRCLE ( 'NONE', #23353, 2.000000000000001776 ) ;
#1537 = VERTEX_POINT ( 'NONE', #25024 ) ;
#1538 = CARTESIAN_POINT ( 'NONE',  ( 36.07789103942399578, -28.20384086642191690, 72.05058123536544201 ) ) ;
#1539 = AXIS2_PLACEMENT_3D ( 'NONE', #8047, #8296, #12174 ) ;
#1540 = EDGE_CURVE ( 'NONE', #13029, #21703, #21191, .T. ) ;
#1541 = CARTESIAN_POINT ( 'NONE',  ( 39.02742774030102879, -28.21368208888610596, 72.26730301774232146 ) ) ;
#1542 = CARTESIAN_POINT ( 'NONE',  ( 40.33642880535524000, -2.313682088886106936, 72.77780686321128201 ) ) ;
#1543 = ORIENTED_EDGE ( 'NONE', *, *, #2231, .T. ) ;
#1544 = DIRECTION ( 'NONE',  ( 3.540251991789399939E-16, 2.999999999999999839E-15, 1.000000000000000000 ) ) ;
#1545 = CARTESIAN_POINT ( 'NONE',  ( 38.73920764526923932, -3.503840866421911393, 70.26206559358664094 ) ) ;
#1546 = DIRECTION ( 'NONE',  ( 0.000000000000000000, -2.999999999999999839E-15, -1.000000000000000000 ) ) ;
#1547 = ORIENTED_EDGE ( 'NONE', *, *, #2650, .T. ) ;
#1548 = FACE_OUTER_BOUND ( 'NONE', #2716, .T. ) ;
#1549 = FACE_OUTER_BOUND ( 'NONE', #339, .T. ) ;
#1550 = CARTESIAN_POINT ( 'NONE',  ( 38.37017380507018771, -11.60384086642191015, 69.04448340153881247 ) ) ;
#1551 = CARTESIAN_POINT ( 'NONE',  ( 36.99021717747880444, -21.72411701483781954, 75.31188971341042304 ) ) ;
#1552 = CARTESIAN_POINT ( 'NONE',  ( 41.14099152588522657, -10.60718113818700026, 84.30501292737000085 ) ) ;
#1553 = CARTESIAN_POINT ( 'NONE',  ( 38.37017380507020192, -16.01368208888610667, 73.11602215082116629 ) ) ;
#1554 = CARTESIAN_POINT ( 'NONE',  ( 33.31606138205700773, 7.864187680719676443, 65.89022736311019912 ) ) ;
#1555 = EDGE_CURVE ( 'NONE', #18393, #21009, #3531, .T. ) ;
#1556 = CARTESIAN_POINT ( 'NONE',  ( 35.31606138205700773, 7.283211578144648257, 66.04722806671131252 ) ) ;
#1557 = VECTOR ( 'NONE', #8982, 1000.000000000000000 ) ;
#1558 = ORIENTED_EDGE ( 'NONE', *, *, #20114, .F. ) ;
#1559 = AXIS2_PLACEMENT_3D ( 'NONE', #18264, #6280, #592 ) ;
#1560 = CARTESIAN_POINT ( 'NONE',  ( 32.56606138205700773, 40.70347903359284913, 83.30501292736984453 ) ) ;
#1561 = CARTESIAN_POINT ( 'NONE',  ( 38.82593461698264292, -10.70384086642191690, 73.13360434286904876 ) ) ;
#1562 = PRODUCT_CONTEXT ( 'NONE', #16705, 'mechanical' ) ;
#1563 = PLANE ( 'NONE',  #17422 ) ;
#1564 = CARTESIAN_POINT ( 'NONE',  ( 36.87297107704152666, -15.71368208888610596, 72.49904802271740323 ) ) ;
#1565 = DIRECTION ( 'NONE',  ( 0.2672894156317878744, -0.9636162972320556630, 3.318080997173179155E-15 ) ) ;
#1566 = CARTESIAN_POINT ( 'NONE',  ( 39.82603832034400426, -21.30384086642191122, 70.35351908239857721 ) ) ;
#1567 = CARTESIAN_POINT ( 'NONE',  ( 33.31606138205700773, 3.536347952325769040, 64.10938348997790115 ) ) ;
#1568 = CARTESIAN_POINT ( 'NONE',  ( 37.80618814713140097, -19.91368208888610170, 73.13360434286903455 ) ) ;
#1569 = ORIENTED_EDGE ( 'NONE', *, *, #14152, .T. ) ;
#1570 = CARTESIAN_POINT ( 'NONE',  ( 36.11133435605973574, -23.61368208888610098, 72.15350918040381600 ) ) ;
#1571 = EDGE_LOOP ( 'NONE', ( #19061, #21109, #19759, #17406 ) ) ;
#1572 = CARTESIAN_POINT ( 'NONE',  ( 31.81606138205700418, 35.95440708241085304, 61.30501292736990138 ) ) ;
#1573 = CYLINDRICAL_SURFACE ( 'NONE', #3825, 1.250000000000000888 ) ;
#1574 = CARTESIAN_POINT ( 'NONE',  ( 37.25260217561390874, -22.00384086642191406, 70.97781676520601479 ) ) ;
#1575 = VECTOR ( 'NONE', #11801, 1000.000000000000000 ) ;
#1576 = ORIENTED_EDGE ( 'NONE', *, *, #7200, .F. ) ;
#1577 = VERTEX_POINT ( 'NONE', #1586 ) ;
#1578 = CARTESIAN_POINT ( 'NONE',  ( 36.31606138205702194, -20.02093502212016318, 26.61211107664843212 ) ) ;
#1579 = DIRECTION ( 'NONE',  ( 0.000000000000000000, -0.3299742535180969494, 0.9439899321577399638 ) ) ;
#1580 = DIRECTION ( 'NONE',  ( -1.000000000000000000, -2.999999999999999839E-15, 0.000000000000000000 ) ) ;
#1581 = CARTESIAN_POINT ( 'NONE',  ( 38.26194895904384197, -26.60384086642191903, 73.71602215082113219 ) ) ;
#1582 = EDGE_CURVE ( 'NONE', #24731, #3483, #24567, .T. ) ;
#1583 = VECTOR ( 'NONE', #20621, 1000.000000000000000 ) ;
#1584 = ADVANCED_FACE ( 'NONE', ( #667 ), #6368, .F. ) ;
#1585 = DIRECTION ( 'NONE',  ( 1.000000000000000000, -0.000000000000000000, 0.000000000000000000 ) ) ;
#1586 = CARTESIAN_POINT ( 'NONE',  ( 45.81606138205700063, 40.39281886181299797, 81.75501292736983316 ) ) ;
#1587 = EDGE_LOOP ( 'NONE', ( #12351, #19325, #9251, #4956 ) ) ;
#1588 = VECTOR ( 'NONE', #24821, 1000.000000000000000 ) ;
#1589 = ORIENTED_EDGE ( 'NONE', *, *, #16586, .F. ) ;
#1590 = DIRECTION ( 'NONE',  ( 0.000000000000000000, -1.000000000000000000, 2.999999999999999839E-15 ) ) ;
#1591 = CARTESIAN_POINT ( 'NONE',  ( 44.81606138205700063, -26.74044063519535186, 84.30501292737007191 ) ) ;
#1592 = ORIENTED_EDGE ( 'NONE', *, *, #18681, .F. ) ;
#1593 = CARTESIAN_POINT ( 'NONE',  ( 36.49096545463212493, -26.10384086642190837, 71.32335560751960202 ) ) ;
#1594 = LINE ( 'NONE', #7420, #2985 ) ;
#1595 = CIRCLE ( 'NONE', #11502, 0.4999999999999943379 ) ;
#1596 = EDGE_LOOP ( 'NONE', ( #4066, #21811, #10775, #18023 ) ) ;
#1597 = CARTESIAN_POINT ( 'NONE',  ( 33.31606138205700773, -21.83924545618511104, 28.60179643084731893 ) ) ;
#1598 = EDGE_CURVE ( 'NONE', #15541, #120, #287, .T. ) ;
#1599 = CARTESIAN_POINT ( 'NONE',  ( 29.81606138205697221, -3.542416608809870304, -4.744096181734387407 ) ) ;
#1600 = LINE ( 'NONE', #17593, #4409 ) ;
#1601 = CARTESIAN_POINT ( 'NONE',  ( 39.31564783533279694, -7.303840866421912104, 70.72433947564853440 ) ) ;
#1602 = AXIS2_PLACEMENT_3D ( 'NONE', #22754, #16570, #1242 ) ;
#1603 = ORIENTED_EDGE ( 'NONE', *, *, #4465, .F. ) ;
#1604 = CARTESIAN_POINT ( 'NONE',  ( 29.81606138205696155, -0.7562224151693598406, -1.633662118351544734 ) ) ;
#1605 = EDGE_LOOP ( 'NONE', ( #92, #20381, #12875, #10899 ) ) ;
#1606 = ORIENTED_EDGE ( 'NONE', *, *, #898, .F. ) ;
#1607 = DIRECTION ( 'NONE',  ( 2.122643018205885151E-17, -1.000000000000000000, 3.120611096041553009E-15 ) ) ;
#1608 = AXIS2_PLACEMENT_3D ( 'NONE', #10658, #22875, #18507 ) ;
#1609 = CARTESIAN_POINT ( 'NONE',  ( 37.60469502381300089, -15.21368208888610063, 70.49320253461759478 ) ) ;
#1610 = CARTESIAN_POINT ( 'NONE',  ( 37.31647492878122563, -13.31368208888610205, 70.72433947564853440 ) ) ;
#1611 = ORIENTED_EDGE ( 'NONE', *, *, #17429, .F. ) ;
#1612 = VERTEX_POINT ( 'NONE', #19892 ) ;
#1613 = DIRECTION ( 'NONE',  ( 2.690219486203388234E-15, -0.8967398287344627850, -0.4425581086832399147 ) ) ;
#1614 = ORIENTED_EDGE ( 'NONE', *, *, #11768, .T. ) ;
#1615 = FACE_OUTER_BOUND ( 'NONE', #21424, .T. ) ;
#1616 = CARTESIAN_POINT ( 'NONE',  ( 37.33957961208645315, -17.80384086642190766, 69.94417936956672577 ) ) ;
#1617 = CARTESIAN_POINT ( 'NONE',  ( 42.99670445188912282, 2.835726111602991040, 6.100265081570795722 ) ) ;
#1618 = CARTESIAN_POINT ( 'NONE',  ( 37.69225076346193504, -15.81368208888610205, 72.33091598616826445 ) ) ;
#1619 = CIRCLE ( 'NONE', #4529, 0.7500000000000001110 ) ;
#1620 = ORIENTED_EDGE ( 'NONE', *, *, #12683, .T. ) ;
#1621 = DIRECTION ( 'NONE',  ( 0.000000000000000000, 0.3299742535180963943, -0.9439899321577402969 ) ) ;
#1622 = DIRECTION ( 'NONE',  ( 1.000000000000000000, 2.065146995210479765E-16, -1.734723475976814737E-16 ) ) ;
#1623 = DIRECTION ( 'NONE',  ( 0.000000000000000000, -1.000000000000000000, 0.000000000000000000 ) ) ;
#1624 = VECTOR ( 'NONE', #6871, 1000.000000000000000 ) ;
#1625 = CARTESIAN_POINT ( 'NONE',  ( 40.31606138205700773, -7.074889544382876316, 83.14300977595306108 ) ) ;
#1626 = FACE_OUTER_BOUND ( 'NONE', #15605, .T. ) ;
#1627 = EDGE_CURVE ( 'NONE', #9965, #22735, #22195, .T. ) ;
#1628 = CARTESIAN_POINT ( 'NONE',  ( 43.81606138205700063, -2.088476903695762665, 19.19551655256602984 ) ) ;
#1629 = ORIENTED_EDGE ( 'NONE', *, *, #3717, .T. ) ;
#1630 = CARTESIAN_POINT ( 'NONE',  ( 43.31606138205700063, -10.93995761290683255, 80.99653337025984001 ) ) ;
#1631 = CARTESIAN_POINT ( 'NONE',  ( 29.81606138205697221, -3.542416608809870304, -4.744096181734387407 ) ) ;
#1632 = ORIENTED_EDGE ( 'NONE', *, *, #9283, .T. ) ;
#1633 = EDGE_LOOP ( 'NONE', ( #3458, #9690, #15478, #1507 ) ) ;
#1634 = CARTESIAN_POINT ( 'NONE',  ( 37.50301148336529877, -8.503840866421917610, 73.69843995877330656 ) ) ;
#1635 = AXIS2_PLACEMENT_3D ( 'NONE', #25363, #15341, #3873 ) ;
#1636 = PLANE ( 'NONE',  #3783 ) ;
#1637 = CARTESIAN_POINT ( 'NONE',  ( 37.80618814713140097, -11.91368208888611058, 73.13360434286903455 ) ) ;
#1638 = VECTOR ( 'NONE', #3573, 1000.000000000000000 ) ;
#1639 = EDGE_LOOP ( 'NONE', ( #23437, #3806, #3552, #24900, #2360, #12605 ) ) ;
#1640 = DIRECTION ( 'NONE',  ( -2.312964634635742267E-15, 0.8967398287344634511, 0.4425581086832385824 ) ) ;
#1641 = FACE_OUTER_BOUND ( 'NONE', #23272, .T. ) ;
#1642 = CARTESIAN_POINT ( 'NONE',  ( 36.29569395875879678, -19.31368208888610027, 69.98269868914867686 ) ) ;
#1643 = AXIS2_PLACEMENT_3D ( 'NONE', #20107, #18312, #377 ) ;
#1644 = VERTEX_POINT ( 'NONE', #8551 ) ;
#1645 = CARTESIAN_POINT ( 'NONE',  ( 38.31606138205700063, 39.69123852234599781, 75.30501292737004349 ) ) ;
#1646 = FACE_OUTER_BOUND ( 'NONE', #1724, .T. ) ;
#1647 = CARTESIAN_POINT ( 'NONE',  ( 31.91606138205697363, -4.349482454670880571, -5.142398479549302515 ) ) ;
#1648 = VECTOR ( 'NONE', #872, 1000.000000000000000 ) ;
#1649 = LINE ( 'NONE', #19193, #18066 ) ;
#1650 = EDGE_CURVE ( 'NONE', #12300, #7324, #14225, .T. ) ;
#1651 = DIRECTION ( 'NONE',  ( -3.469446951953616555E-15, 0.8967398287344632291, 0.4425581086832389155 ) ) ;
#1652 = AXIS2_PLACEMENT_3D ( 'NONE', #11685, #11808, #15407 ) ;
#1653 = CARTESIAN_POINT ( 'NONE',  ( 37.69225076346193504, -11.80384086642191477, 70.42958956619168021 ) ) ;
#1654 = CARTESIAN_POINT ( 'NONE',  ( 38.93415946300897446, -2.113682088886109423, 73.09843995877331224 ) ) ;
#1655 = ORIENTED_EDGE ( 'NONE', *, *, #17523, .T. ) ;
#1656 = LINE ( 'NONE', #5419, #7800 ) ;
#1657 = LINE ( 'NONE', #23301, #818 ) ;
#1658 = VERTEX_POINT ( 'NONE', #2351 ) ;
#1659 = ORIENTED_EDGE ( 'NONE', *, *, #10742, .T. ) ;
#1660 = CARTESIAN_POINT ( 'NONE',  ( 38.37017380507018771, 0.3961591335780931256, 69.64448340153880679 ) ) ;
#1661 = CARTESIAN_POINT ( 'NONE',  ( 39.29254315202756231, 1.186317911113898838, 69.94417936956675419 ) ) ;
#1662 = PRODUCT ( 'Upper Tension Leaf Spring', 'Upper Tension Leaf Spring', '', ( #1562 ) ) ;
#1663 = CARTESIAN_POINT ( 'NONE',  ( 39.64521430340304420, -0.8136820888860993861, 69.45876917294177133 ) ) ;
#1664 = EDGE_LOOP ( 'NONE', ( #7698, #19659, #15384, #19509 ) ) ;
#1665 = CARTESIAN_POINT ( 'NONE',  ( 36.31606138205700063, 42.19123852234599781, 74.30501292736987295 ) ) ;
#1666 = CARTESIAN_POINT ( 'NONE',  ( 37.25260217561390874, -8.003840866421910505, 70.97781676520604321 ) ) ;
#1667 = EDGE_CURVE ( 'NONE', #5253, #2986, #2770, .T. ) ;
#1668 = DIRECTION ( 'NONE',  ( -1.734723475976804876E-16, -3.491481338843135327E-15, -1.000000000000000000 ) ) ;
#1669 = ADVANCED_FACE ( 'NONE', ( #544 ), #17198, .T. ) ;
#1670 = EDGE_LOOP ( 'NONE', ( #19907, #18202, #22450, #14186 ) ) ;
#1671 = LINE ( 'NONE', #25110, #14190 ) ;
#1672 = LINE ( 'NONE', #11757, #23163 ) ;
#1673 = CARTESIAN_POINT ( 'NONE',  ( 37.50301148336529877, -8.503840866421917610, 73.69843995877330656 ) ) ;
#1674 = EDGE_CURVE ( 'NONE', #5806, #9258, #2099, .T. ) ;
#1675 = ADVANCED_FACE ( 'NONE', ( #414 ), #8427, .F. ) ;
#1676 = EDGE_CURVE ( 'NONE', #14477, #21091, #11447, .T. ) ;
#1677 = LINE ( 'NONE', #21275, #16046 ) ;
#1678 = SURFACE_STYLE_FILL_AREA ( #9947 ) ;
#1679 = CARTESIAN_POINT ( 'NONE',  ( 38.37017380507020192, -12.01368208888610845, 73.11602215082116629 ) ) ;
#1680 = CARTESIAN_POINT ( 'NONE',  ( 33.91846891627784544, 2.749301080711977985, 6.091107676698986673 ) ) ;
#1681 = ORIENTED_EDGE ( 'NONE', *, *, #10661, .T. ) ;
#1682 = DIRECTION ( 'NONE',  ( 0.000000000000000000, 0.8212051873014208914, 0.5706330172266919076 ) ) ;
#1683 = EDGE_CURVE ( 'NONE', #18636, #16606, #16266, .T. ) ;
#1684 = CARTESIAN_POINT ( 'NONE',  ( 37.80618814713138676, -7.703840866421908906, 69.62690120949091011 ) ) ;
#1686 = EDGE_CURVE ( 'NONE', #4506, #22728, #20142, .T. ) ;
#1685 = APPLICATION_PROTOCOL_DEFINITION ( 'draft international standard', 'automotive_design', 1998, #15233 ) ;
#1687 = DIRECTION ( 'NONE',  ( 0.000000000000000000, 0.5706330172266920187, -0.8212051873014210024 ) ) ;
#1688 = CARTESIAN_POINT ( 'NONE',  ( 39.75915168707250302, -20.71368208888610596, 70.26145752964251301 ) ) ;
#1689 = CYLINDRICAL_SURFACE ( 'NONE', #24607, 1.750000000000001554 ) ;
#1690 = CARTESIAN_POINT ( 'NONE',  ( 39.75915168707251723, -16.90384086642191619, 72.49904802271738902 ) ) ;
#1691 = CARTESIAN_POINT ( 'NONE',  ( 36.72255525790973252, -5.988568098966074338, 83.27624199006054084 ) ) ;
#1692 = EDGE_CURVE ( 'NONE', #4589, #20194, #18093, .T. ) ;
#1693 = VECTOR ( 'NONE', #3885, 999.9999999999998863 ) ;
#1694 = CARTESIAN_POINT ( 'NONE',  ( 40.14115730948191185, -20.51368208888609601, 71.32335560751960202 ) ) ;
#1695 = ORIENTED_EDGE ( 'NONE', *, *, #19017, .F. ) ;
#1696 = CARTESIAN_POINT ( 'NONE',  ( 39.02088643472237095, -22.91368208888609814, 69.02690120949091579 ) ) ;
#1697 = ORIENTED_EDGE ( 'NONE', *, *, #18160, .T. ) ;
#1698 = CARTESIAN_POINT ( 'NONE',  ( 43.06606138205700063, 43.19123852234599781, 74.30501292736987295 ) ) ;
#1699 = DIRECTION ( 'NONE',  ( 1.000000000000000000, 0.000000000000000000, 0.000000000000000000 ) ) ;
#1700 = CARTESIAN_POINT ( 'NONE',  ( 37.21915885897815457, -22.20384086642191335, 71.67976084211552745 ) ) ;
#1701 = VERTEX_POINT ( 'NONE', #18342 ) ;
#1702 = EDGE_LOOP ( 'NONE', ( #16971, #18877, #24015, #20126 ) ) ;
#1703 = DIRECTION ( 'NONE',  ( -1.000000000000000000, -2.411023719125726758E-15, -1.389056744264227588E-15 ) ) ;
#1704 = CARTESIAN_POINT ( 'NONE',  ( 45.81606138205697221, -3.984974717493084739, -3.847356352999882656 ) ) ;
#1705 = EDGE_LOOP ( 'NONE', ( #1408, #19201, #23703, #1204 ) ) ;
#1706 = CYLINDRICAL_SURFACE ( 'NONE', #23794, 1.750000000000001554 ) ;
#1707 = CARTESIAN_POINT ( 'NONE',  ( 37.33957961208645315, 0.1961591335780908663, 69.94417936956673998 ) ) ;
#1708 = CARTESIAN_POINT ( 'NONE',  ( 43.06606138205700063, 43.19123852234599070, 73.55501292736987295 ) ) ;
#1709 = CARTESIAN_POINT ( 'NONE',  ( 38.31606138205700063, -4.399276463885007260, 59.51717649063222382 ) ) ;
#1710 = VECTOR ( 'NONE', #11846, 1000.000000000000227 ) ;
#1711 = VERTEX_POINT ( 'NONE', #15887 ) ;
#1712 = ORIENTED_EDGE ( 'NONE', *, *, #6965, .F. ) ;
#1713 = APPLICATION_CONTEXT ( 'automotive_design' ) ;
#1714 = DIRECTION ( 'NONE',  ( 0.000000000000000000, -2.999999999999999839E-15, -1.000000000000000000 ) ) ;
#1715 = FACE_OUTER_BOUND ( 'NONE', #18455, .T. ) ;
#1716 = CIRCLE ( 'NONE', #3370, 1.499999999999999778 ) ;
#1717 = CARTESIAN_POINT ( 'NONE',  ( 36.80608444377002542, -28.30384086642191122, 72.40698646996131060 ) ) ;
#1718 = CARTESIAN_POINT ( 'NONE',  ( 36.31606138205700773, -19.92642959707778516, 24.72592537066031682 ) ) ;
#1719 = ORIENTED_EDGE ( 'NONE', *, *, #7493, .T. ) ;
#1720 = DIRECTION ( 'NONE',  ( -1.000000000000000000, -2.556434596176347380E-15, -1.460819769243627131E-15 ) ) ;
#1721 = DIRECTION ( 'NONE',  ( 1.000000000000000000, 0.000000000000000000, 0.000000000000000000 ) ) ;
#1722 = CYLINDRICAL_SURFACE ( 'NONE', #2331, 3.000000000000002665 ) ;
#1723 = CARTESIAN_POINT ( 'NONE',  ( 37.31647492878124694, -6.303840866421912104, 72.03616607671141026 ) ) ;
#1724 = EDGE_LOOP ( 'NONE', ( #1878, #5691, #21493, #16540 ) ) ;
#1725 = ADVANCED_FACE ( 'NONE', ( #4177 ), #13962, .T. ) ;
#1726 = DIRECTION ( 'NONE',  ( 0.000000000000000000, 1.000000000000000000, -4.625929269271481378E-15 ) ) ;
#1727 = VERTEX_POINT ( 'NONE', #20013 ) ;
#1728 = ADVANCED_FACE ( 'NONE', ( #2604 ), #23989, .F. ) ;
#1729 = ORIENTED_EDGE ( 'NONE', *, *, #4047, .T. ) ;
#1730 = VECTOR ( 'NONE', #2169, 1000.000000000000000 ) ;
#1731 = PLANE ( 'NONE',  #18014 ) ;
#1732 = CARTESIAN_POINT ( 'NONE',  ( 38.93987200065208754, -10.81368208888610027, 70.42958956619168021 ) ) ;
#1733 = CARTESIAN_POINT ( 'NONE',  ( 39.02742774030102879, -8.213682088886098853, 72.26730301774236409 ) ) ;
#1734 = EDGE_LOOP ( 'NONE', ( #185, #8919, #11633, #24570, #11697, #17570, #604, #9185, #598, #6119, #12537, #16413, #3459 ) ) ;
#1735 = ORIENTED_EDGE ( 'NONE', *, *, #22580, .T. ) ;
#1736 = DIRECTION ( 'NONE',  ( -1.327674326049719602E-15, 0.4425581086832399147, -0.8967398287344627850 ) ) ;
#1737 = AXIS2_PLACEMENT_3D ( 'NONE', #20070, #12488, #3306 ) ;
#1738 = DIRECTION ( 'NONE',  ( 0.000000000000000000, -2.999999999999999839E-15, -1.000000000000000000 ) ) ;
#1739 = VERTEX_POINT ( 'NONE', #16385 ) ;
#1740 = CYLINDRICAL_SURFACE ( 'NONE', #8286, 3.999999999999996447 ) ;
#1741 = CARTESIAN_POINT ( 'NONE',  ( 40.14115730948191185, -19.10384086642191193, 71.43714994484030001 ) ) ;
#1742 = FACE_OUTER_BOUND ( 'NONE', #23140, .T. ) ;
#1743 = VECTOR ( 'NONE', #5542, 1000.000000000000000 ) ;
#1744 = VECTOR ( 'NONE', #6544, 1000.000000000000000 ) ;
#1745 = CARTESIAN_POINT ( 'NONE',  ( 39.37952058850012804, -20.61368208888610098, 70.97781676520601479 ) ) ;
#1746 = ORIENTED_EDGE ( 'NONE', *, *, #21067, .T. ) ;
#1747 = DIRECTION ( 'NONE',  ( 0.000000000000000000, 0.000000000000000000, 1.000000000000000000 ) ) ;
#1748 = CARTESIAN_POINT ( 'NONE',  ( 36.49096545463212493, -15.51368208888610667, 71.43714994484034264 ) ) ;
#1749 = AXIS2_PLACEMENT_3D ( 'NONE', #22322, #6608, #14002 ) ;
#1750 = DIRECTION ( 'NONE',  ( -1.000000000000000000, -4.949452455753099023E-16, 7.122819585028524934E-16 ) ) ;
#1751 = CIRCLE ( 'NONE', #15334, 1.000000000000000888 ) ;
#1752 = DIRECTION ( 'NONE',  ( 0.000000000000000000, -0.5706330172266907974, 0.8212051873014217795 ) ) ;
#1753 = CARTESIAN_POINT ( 'NONE',  ( 38.83610899671118943, -5.268488250605326328, 83.30484769703562620 ) ) ;
#1754 = DIRECTION ( 'NONE',  ( 3.965082230804126670E-15, -0.8967398287344626739, -0.4425581086832401922 ) ) ;
#1755 = AXIS2_PLACEMENT_3D ( 'NONE', #3524, #11786, #21303 ) ;
#1756 = EDGE_CURVE ( 'NONE', #3936, #14994, #21690, .T. ) ;
#1757 = DIRECTION ( 'NONE',  ( 1.000000000000000000, 3.091505625455828697E-15, 4.515976121274772923E-17 ) ) ;
#1758 = ADVANCED_FACE ( 'NONE', ( #19758 ), #5194, .F. ) ;
#1759 = ORIENTED_EDGE ( 'NONE', *, *, #12427, .T. ) ;
#1760 = AXIS2_PLACEMENT_3D ( 'NONE', #16947, #3023, #830 ) ;
#1761 = EDGE_CURVE ( 'NONE', #19667, #17699, #12931, .T. ) ;
#1762 = CARTESIAN_POINT ( 'NONE',  ( 34.81606138205697221, -3.103162021984047669, -5.046558096268735305 ) ) ;
#1763 = ORIENTED_EDGE ( 'NONE', *, *, #12811, .F. ) ;
#1764 = ORIENTED_EDGE ( 'NONE', *, *, #2611, .T. ) ;
#1765 = CARTESIAN_POINT ( 'NONE',  ( 36.98690846071097127, -7.803840866421912104, 69.45876917294177133 ) ) ;
#1766 = MECHANICAL_DESIGN_GEOMETRIC_PRESENTATION_REPRESENTATION (  '', ( #17014 ), #3838 ) ;
#1767 = ORIENTED_EDGE ( 'NONE', *, *, #23665, .F. ) ;
#1768 = LINE ( 'NONE', #21494, #19414 ) ;
#1769 = CARTESIAN_POINT ( 'NONE',  ( 36.80608444377001121, -13.31368208888609672, 70.35351908239857721 ) ) ;
#1770 = AXIS2_PLACEMENT_3D ( 'NONE', #4688, #22333, #14849 ) ;
#1771 =( LENGTH_UNIT ( ) NAMED_UNIT ( * ) SI_UNIT ( .MILLI., .METRE. ) );
#1772 = ORIENTED_EDGE ( 'NONE', *, *, #6265, .T. ) ;
#1773 = FACE_OUTER_BOUND ( 'NONE', #6985, .T. ) ;
#1774 = DIRECTION ( 'NONE',  ( -0.000000000000000000, -1.000000000000000000, 2.848211695852029218E-15 ) ) ;
#1775 = EDGE_CURVE ( 'NONE', #8838, #3808, #2852, .T. ) ;
#1776 = AXIS2_PLACEMENT_3D ( 'NONE', #23319, #11499, #23452 ) ;
#1777 = CARTESIAN_POINT ( 'NONE',  ( 38.37017380507020192, -22.01368208888611022, 73.71602215082113219 ) ) ;
#1778 = ORIENTED_EDGE ( 'NONE', *, *, #18713, .F. ) ;
#1779 = FACE_OUTER_BOUND ( 'NONE', #18015, .T. ) ;
#1780 = CARTESIAN_POINT ( 'NONE',  ( 36.81465384343994884, 41.67000142393845152, 79.57823623207323749 ) ) ;
#1781 = DIRECTION ( 'NONE',  ( 0.000000000000000000, -2.999999999999999839E-15, -1.000000000000000000 ) ) ;
#1782 = AXIS2_PLACEMENT_3D ( 'NONE', #13346, #1714, #17204 ) ;
#1783 = CARTESIAN_POINT ( 'NONE',  ( 35.81606138205700063, -29.78523130861184498, 52.92072663988442116 ) ) ;
#1784 =( GEOMETRIC_REPRESENTATION_CONTEXT ( 3 ) GLOBAL_UNCERTAINTY_ASSIGNED_CONTEXT ( ( #24188 ) ) GLOBAL_UNIT_ASSIGNED_CONTEXT ( ( #11078, #5403, #24948 ) ) REPRESENTATION_CONTEXT ( 'NONE', 'WORKASPACE' ) );
#1785 = CIRCLE ( 'NONE', #13752, 3.999999999999997335 ) ;
#1786 = CARTESIAN_POINT ( 'NONE',  ( 36.36697178183959522, -6.685332804587225120, 83.20286675510105567 ) ) ;
#1787 = CARTESIAN_POINT ( 'NONE',  ( 37.21915885897815457, -12.20384086642191157, 71.67976084211552745 ) ) ;
#1788 = CARTESIAN_POINT ( 'NONE',  ( 37.69796330110504101, 0.8863179111139003474, 69.66206559358664663 ) ) ;
#1789 = ORIENTED_EDGE ( 'NONE', *, *, #10064, .F. ) ;
#1790 = CARTESIAN_POINT ( 'NONE',  ( 38.58006293444520196, -22.20877047264255921, 75.80998976194723582 ) ) ;
#1791 = VECTOR ( 'NONE', #10771, 1000.000000000000000 ) ;
#1792 = LINE ( 'NONE', #17788, #13583 ) ;
#1793 = VERTEX_POINT ( 'NONE', #4682 ) ;
#1794 = ORIENTED_EDGE ( 'NONE', *, *, #22157, .T. ) ;
#1795 = CARTESIAN_POINT ( 'NONE',  ( 39.95015449827720744, -1.003840866421912281, 71.96809898377888715 ) ) ;
#1796 = CARTESIAN_POINT ( 'NONE',  ( 39.38009889167650357, -0.2136820888861065693, 72.75271321436733274 ) ) ;
#1797 = CARTESIAN_POINT ( 'NONE',  ( 39.12911128074873801, -4.113682088886107202, 73.69843995877330656 ) ) ;
#1798 = ORIENTED_EDGE ( 'NONE', *, *, #18346, .T. ) ;
#1799 = DIRECTION ( 'NONE',  ( -1.000000000000000000, -1.052872940142565459E-15, -1.848188032574765003E-17 ) ) ;
#1800 = CARTESIAN_POINT ( 'NONE',  ( 37.69225076346193504, -3.803840866421912992, 70.42958956619168021 ) ) ;
#1801 = DIRECTION ( 'NONE',  ( -1.000000000000000000, 0.000000000000000000, 0.000000000000000000 ) ) ;
#1802 = ORIENTED_EDGE ( 'NONE', *, *, #9504, .F. ) ;
#1803 = PLANE ( 'NONE',  #18725 ) ;
#1804 = PLANE ( 'NONE',  #19891 ) ;
#1805 = ADVANCED_FACE ( 'NONE', ( #22575 ), #20906, .F. ) ;
#1806 = CARTESIAN_POINT ( 'NONE',  ( 37.50301148336529877, -12.50384086642191939, 73.69843995877327814 ) ) ;
#1807 = AXIS2_PLACEMENT_3D ( 'NONE', #21939, #14085, #12169 ) ;
#1808 = VECTOR ( 'NONE', #12372, 1000.000000000000227 ) ;
#1809 = DIRECTION ( 'NONE',  ( -1.292451913828718831E-15, 0.4425581086832399147, -0.8967398287344627850 ) ) ;
#1810 = LINE ( 'NONE', #17806, #24738 ) ;
#1811 = CARTESIAN_POINT ( 'NONE',  ( 37.69796330110504101, -11.11368208888610276, 69.66206559358663242 ) ) ;
#1812 = CARTESIAN_POINT ( 'NONE',  ( 35.31606138205700773, 7.043113989679085307, 66.83274420321491505 ) ) ;
#1813 = VECTOR ( 'NONE', #15382, 1000.000000000000000 ) ;
#1814 = CARTESIAN_POINT ( 'NONE',  ( 46.81606138205706458, -34.13844651005145181, 70.48338531520533934 ) ) ;
#1815 = ORIENTED_EDGE ( 'NONE', *, *, #14904, .T. ) ;
#1816 = DIRECTION ( 'NONE',  ( -1.000000000000000000, 0.000000000000000000, 0.000000000000000000 ) ) ;
#1817 = CARTESIAN_POINT ( 'NONE',  ( 37.33957961208645315, -3.803840866421909439, 69.94417936956673998 ) ) ;
#1818 = ITEM_DEFINED_TRANSFORMATION ( 'NONE', 'NONE', #9672,  #2000 ) ;
#1819 = CARTESIAN_POINT ( 'NONE',  ( 43.23147868389327897, 40.76768529863396395, 79.37823623207322044 ) ) ;
#1820 = EDGE_CURVE ( 'NONE', #24841, #1075, #6741, .T. ) ;
#1821 = CARTESIAN_POINT ( 'NONE',  ( 38.37017380507020192, -18.01368208888611022, 73.11602215082116629 ) ) ;
#1822 = AXIS2_PLACEMENT_3D ( 'NONE', #18348, #20790, #6747 ) ;
#1823 = EDGE_CURVE ( 'NONE', #20324, #10597, #10869, .T. ) ;
#1824 = DIRECTION ( 'NONE',  ( -1.000000000000000000, -2.751104698760144965E-15, 1.228345504986737969E-16 ) ) ;
#1825 = CARTESIAN_POINT ( 'NONE',  ( 39.38009889167648936, -15.40384086642190908, 70.00779233799262613 ) ) ;
#1826 = EDGE_CURVE ( 'NONE', #13483, #15432, #7333, .T. ) ;
#1827 = DIRECTION ( 'NONE',  ( 0.000000000000000000, 0.7540134720837716742, 0.6568589528324746407 ) ) ;
#1828 = CARTESIAN_POINT ( 'NONE',  ( 39.82603832034400426, -16.31368208888610738, 72.40698646996133903 ) ) ;
#1829 = ORIENTED_EDGE ( 'NONE', *, *, #2608, .T. ) ;
#1830 = CARTESIAN_POINT ( 'NONE',  ( 40.33642880535524000, -22.31368208888610738, 72.77780686321126780 ) ) ;
#1831 = ORIENTED_EDGE ( 'NONE', *, *, #1531, .F. ) ;
#1832 = CARTESIAN_POINT ( 'NONE',  ( 45.81606138205697221, -3.542416608809821454, -4.744096181734387407 ) ) ;
#1833 = LINE ( 'NONE', #11394, #15762 ) ;
#1834 = CARTESIAN_POINT ( 'NONE',  ( 38.73920764526923932, -23.50384086642191050, 70.26206559358661252 ) ) ;
#1835 = VERTEX_POINT ( 'NONE', #11120 ) ;
#1836 = ORIENTED_EDGE ( 'NONE', *, *, #15903, .T. ) ;
#1837 = CARTESIAN_POINT ( 'NONE',  ( 39.61574158285312564, -28.86380355457609070, 70.74205085096339474 ) ) ;
#1838 = CARTESIAN_POINT ( 'NONE',  ( 31.81606138205700418, -11.72563467517899838, 72.98595903681224684 ) ) ;
#1839 = ORIENTED_EDGE ( 'NONE', *, *, #24052, .F. ) ;
#1840 = EDGE_CURVE ( 'NONE', #8848, #12037, #13918, .T. ) ;
#1841 = LINE ( 'NONE', #11533, #13931 ) ;
#1842 = CARTESIAN_POINT ( 'NONE',  ( 37.80618814713138676, 0.2961591335780937584, 69.62690120949091011 ) ) ;
#1843 = LINE ( 'NONE', #23311, #11133 ) ;
#1844 = CARTESIAN_POINT ( 'NONE',  ( 39.12911128074873801, -2.113682088886108534, 73.69843995877330656 ) ) ;
#1845 = DIRECTION ( 'NONE',  ( -1.218693434051482139E-16, 0.4425581086832393041, -0.8967398287344630070 ) ) ;
#1846 = CIRCLE ( 'NONE', #16246, 0.5000000000000004441 ) ;
#1847 = ORIENTED_EDGE ( 'NONE', *, *, #19132, .T. ) ;
#1848 = VERTEX_POINT ( 'NONE', #17046 ) ;
#1849 = DIRECTION ( 'NONE',  ( -1.734723475976804876E-16, -3.469446951953610245E-15, -1.000000000000000000 ) ) ;
#1850 = DIRECTION ( 'NONE',  ( 1.133678928659556219E-16, -0.4425581086832399147, 0.8967398287344627850 ) ) ;
#1851 = CARTESIAN_POINT ( 'NONE',  ( 36.68196826583682935, -20.00384086642191050, 70.79240656858107172 ) ) ;
#1852 = DIRECTION ( 'NONE',  ( -2.690219486203387839E-15, 0.8967398287344625629, 0.4425581086832404143 ) ) ;
#1853 = ORIENTED_EDGE ( 'NONE', *, *, #1903, .F. ) ;
#1854 = CARTESIAN_POINT ( 'NONE',  ( 38.41621794735363693, -36.60729675983900222, 83.30501292737011454 ) ) ;
#1855 = CARTESIAN_POINT ( 'NONE',  ( 43.80758610329830560, -33.17626767724734549, 59.69730752409159180 ) ) ;
#1856 = CARTESIAN_POINT ( 'NONE',  ( 40.31606138205699352, -10.61256217995207685, 37.48782943861662886 ) ) ;
#1857 = ADVANCED_FACE ( 'NONE', ( #795 ), #12802, .F. ) ;
#1858 = CARTESIAN_POINT ( 'NONE',  ( 38.73920764526923932, -3.503840866421911393, 70.26206559358664094 ) ) ;
#1859 = EDGE_CURVE ( 'NONE', #16267, #9779, #14977, .T. ) ;
#1860 = ORIENTED_EDGE ( 'NONE', *, *, #12473, .T. ) ;
#1861 = CARTESIAN_POINT ( 'NONE',  ( 43.81606138205700063, 6.699978067258562042, 7.424159817622362212 ) ) ;
#1862 = EDGE_LOOP ( 'NONE', ( #9658, #372, #668, #7998 ) ) ;
#1863 = EDGE_LOOP ( 'NONE', ( #8870, #16728, #13570, #6462, #11014 ) ) ;
#1864 = DIRECTION ( 'NONE',  ( 1.000000000000000000, 0.000000000000000000, 0.000000000000000000 ) ) ;
#1865 = CARTESIAN_POINT ( 'NONE',  ( 39.02742774030102879, -12.21368208888610063, 72.26730301774234988 ) ) ;
#1866 = CARTESIAN_POINT ( 'NONE',  ( 38.63098279924288647, -8.913682088886103472, 70.22690120949091863 ) ) ;
#1867 = ORIENTED_EDGE ( 'NONE', *, *, #17709, .T. ) ;
#1868 = ORIENTED_EDGE ( 'NONE', *, *, #21287, .F. ) ;
#1869 = DIRECTION ( 'NONE',  ( -0.000000000000000000, -3.469446951953613400E-15, -1.000000000000000000 ) ) ;
#1870 = LINE ( 'NONE', #17869, #4225 ) ;
#1871 = ORIENTED_EDGE ( 'NONE', *, *, #114, .T. ) ;
#1872 = ADVANCED_FACE ( 'NONE', ( #22701 ), #10741, .T. ) ;
#1873 = CARTESIAN_POINT ( 'NONE',  ( 43.06606138205700063, -34.55876147765401640, 70.30501292737011454 ) ) ;
#1874 = CARTESIAN_POINT ( 'NONE',  ( 36.49096545463212493, -16.10384086642191548, 71.32335560751961623 ) ) ;
#1875 = CARTESIAN_POINT ( 'NONE',  ( 43.81606138205700063, 35.92314894770293421, 79.37823623207323465 ) ) ;
#1876 = CARTESIAN_POINT ( 'NONE',  ( 38.26194895904383486, -17.01368208888610312, 70.24448340153875847 ) ) ;
#1877 = VERTEX_POINT ( 'NONE', #20646 ) ;
#1878 = ORIENTED_EDGE ( 'NONE', *, *, #18870, .F. ) ;
#1879 = PLANE ( 'NONE',  #4650 ) ;
#1880 = CARTESIAN_POINT ( 'NONE',  ( 39.38009889167650357, -12.21368208888610596, 72.75271321436731853 ) ) ;
#1881 = EDGE_CURVE ( 'NONE', #5254, #8221, #734, .T. ) ;
#1882 = DIRECTION ( 'NONE',  ( 0.000000000000000000, -0.5706330172266919076, 0.8212051873014208914 ) ) ;
#1883 = CARTESIAN_POINT ( 'NONE',  ( 41.81606138205696510, -1.316127829577467656, -4.808842309729777220 ) ) ;
#1884 = DIRECTION ( 'NONE',  ( 0.000000000000000000, -1.000000000000000000, 3.491481338843135327E-15 ) ) ;
#1885 = LINE ( 'NONE', #25193, #4850 ) ;
#1886 = B_SPLINE_SURFACE_WITH_KNOTS ( 'NONE', 1, 3, ( 
 ( #15714, #17656, #1790, #15958, #7735, #23691, #4256, #14041, #15580, #23814, #9682, #13787, #23438, #21896, #12126, #23564 ),
 ( #19703, #2050, #17787, #19968, #2299, #10174, #16089, #12243, #12507, #361, #24310, #6815, #10304, #12376, #6679, #14660 ),
 ( #14542, #8755, #22401, #6437, #8245, #18415, #743, #22524, #6314, #16333, #4628, #4751, #20216, #8499, #4504, #14175 ),
 ( #10559, #4878, #24184, #490, #12756, #2552, #10434, #2929, #24442, #23939, #18537, #22020, #18295, #865, #618, #4381 ) ),
 .UNSPECIFIED., .F., .F., .F.,
 ( 2, 1, 1, 2 ),
 ( 4, 2, 2, 2, 2, 2, 2, 4 ),
 ( -0.01000000000000000021, 0.000000000000000000, 1.000000000000000000, 1.010099999999999998 ),
 ( 0.003140158914087874936, 0.003532297574693944991, 0.003924436235300010276, 0.004316574895906080331, 0.004708713556512150386, 0.005100852217118210033, 0.005492990877724280088, 0.006277268198936420199 ),
 .UNSPECIFIED. ) ;
#1887 = CARTESIAN_POINT ( 'NONE',  ( 44.81606138205700063, 41.44123852234595518, 61.30501292736988006 ) ) ;
#1888 = ORIENTED_EDGE ( 'NONE', *, *, #14158, .T. ) ;
#1889 = CARTESIAN_POINT ( 'NONE',  ( 33.56606138205700773, -34.55876147765400930, 73.55501292737011454 ) ) ;
#1890 = ORIENTED_EDGE ( 'NONE', *, *, #8714, .T. ) ;
#1891 = EDGE_LOOP ( 'NONE', ( #16584, #9694, #23122, #20814 ) ) ;
#1892 = CARTESIAN_POINT ( 'NONE',  ( 39.12911128074872380, -9.503840866421912281, 69.06206559358666652 ) ) ;
#1893 = ORIENTED_EDGE ( 'NONE', *, *, #12474, .F. ) ;
#1894 = DIRECTION ( 'NONE',  ( -1.000000000000000000, 0.000000000000000000, 0.000000000000000000 ) ) ;
#1895 = CARTESIAN_POINT ( 'NONE',  ( 36.64852494920107517, -15.41368208888610525, 70.89533451361947414 ) ) ;
#1896 = ORIENTED_EDGE ( 'NONE', *, *, #14372, .F. ) ;
#1897 = DIRECTION ( 'NONE',  ( 2.690219486203388234E-15, -0.8967398287344627850, -0.4425581086832399147 ) ) ;
#1898 = CARTESIAN_POINT ( 'NONE',  ( 36.06606138205700063, 5.308699250829721272, 2.416607620847027960 ) ) ;
#1899 = CARTESIAN_POINT ( 'NONE',  ( 40.55423172469004811, -18.41368208888610525, 72.05058123536544201 ) ) ;
#1900 = EDGE_LOOP ( 'NONE', ( #6401, #1993 ) ) ;
#1901 = ADVANCED_FACE ( 'NONE', ( #2723 ), #6992, .T. ) ;
#1902 = SURFACE_SIDE_STYLE ('',( #23682 ) ) ;
#1903 = EDGE_CURVE ( 'NONE', #12694, #9681, #8685, .T. ) ;
#1904 = CARTESIAN_POINT ( 'NONE',  ( 46.81606138205697221, -5.918777154956146980, -5.916875169744970187 ) ) ;
#1905 = DIRECTION ( 'NONE',  ( 5.421010862427517856E-17, -0.7540134720837717852, -0.6568589528324746407 ) ) ;
#1906 = EDGE_CURVE ( 'NONE', #10160, #8707, #24745, .T. ) ;
#1907 = ORIENTED_EDGE ( 'NONE', *, *, #13379, .F. ) ;
#1908 = DIRECTION ( 'NONE',  ( 1.000000000000000000, 1.734723475976804876E-16, -1.734723475976814737E-16 ) ) ;
#1909 =( LENGTH_UNIT ( ) NAMED_UNIT ( * ) SI_UNIT ( .MILLI., .METRE. ) );
#1910 = AXIS2_PLACEMENT_3D ( 'NONE', #19470, #15097, #25253 ) ;
#1911 = CARTESIAN_POINT ( 'NONE',  ( 36.31606138205700063, 5.691238522346989903, 65.80501292736998664 ) ) ;
#1912 = DIRECTION ( 'NONE',  ( -1.000000000000000000, 0.000000000000000000, 0.000000000000000000 ) ) ;
#1913 = CARTESIAN_POINT ( 'NONE',  ( 38.93987200065210175, -12.80384086642190944, 72.33091598616826445 ) ) ;
#1914 = CARTESIAN_POINT ( 'NONE',  ( 39.95015449827720744, 1.386317911113894130, 70.79240656858108593 ) ) ;
#1915 = VERTEX_POINT ( 'NONE', #7122 ) ;
#1916 = DIRECTION ( 'NONE',  ( 0.000000000000000000, 0.7540134720837725624, 0.6568589528324736415 ) ) ;
#1917 = CARTESIAN_POINT ( 'NONE',  ( 44.06606138205700063, -26.74044063519535186, 82.55501292737007191 ) ) ;
#1918 = ORIENTED_EDGE ( 'NONE', *, *, #17611, .F. ) ;
#1919 = ORIENTED_EDGE ( 'NONE', *, *, #12872, .F. ) ;
#1920 = CARTESIAN_POINT ( 'NONE',  ( 38.26194895904384197, -28.60384086642191548, 73.71602215082113219 ) ) ;
#1921 = CARTESIAN_POINT ( 'NONE',  ( 38.00113996487114321, -23.91368208888610170, 72.53360434286901182 ) ) ;
#1922 = CARTESIAN_POINT ( 'NONE',  ( 39.73277004305198545, -4.213682088886105959, 73.23812341099225875 ) ) ;
#1923 = CIRCLE ( 'NONE', #5236, 1.000000000000000888 ) ;
#1924 = EDGE_LOOP ( 'NONE', ( #4738, #10941, #16863, #9235 ) ) ;
#1925 = DIRECTION ( 'NONE',  ( -1.000000000000000000, -1.000000000000000078E-15, 0.000000000000000000 ) ) ;
#1926 = VECTOR ( 'NONE', #21980, 1000.000000000000000 ) ;
#1927 = CARTESIAN_POINT ( 'NONE',  ( 39.24876120206129571, -6.903840866421912636, 72.12822762946750288 ) ) ;
#1928 = CIRCLE ( 'NONE', #23314, 3.999999999999899636 ) ;
#1929 = VECTOR ( 'NONE', #6753, 1000.000000000000114 ) ;
#1930 = CARTESIAN_POINT ( 'NONE',  ( 32.81606138205700773, 2.191238522347013440, 73.80501292737000085 ) ) ;
#1931 = ORIENTED_EDGE ( 'NONE', *, *, #5771, .T. ) ;
#1932 = FACE_OUTER_BOUND ( 'NONE', #21271, .T. ) ;
#1933 = DIRECTION ( 'NONE',  ( -1.327674326049719602E-15, 0.4425581086832399147, -0.8967398287344627850 ) ) ;
#1934 = CARTESIAN_POINT ( 'NONE',  ( 40.55423172469004101, -11.20384086642191690, 70.70992431699450265 ) ) ;
#1935 = DIRECTION ( 'NONE',  ( -1.000000000000000000, -3.091505625455828697E-15, -4.515976121274772923E-17 ) ) ;
#1936 = PRESENTATION_STYLE_ASSIGNMENT (( #13426 ) ) ;
#1937 = CARTESIAN_POINT ( 'NONE',  ( 39.82603832034400426, -12.31368208888610560, 72.40698646996133903 ) ) ;
#1938 = CARTESIAN_POINT ( 'NONE',  ( 34.06606138205700773, 2.736744647373095418, 6.109177798617293931 ) ) ;
#1939 = CARTESIAN_POINT ( 'NONE',  ( 42.96606138205694236, 5.208890205473748480, 5.429380561359602453 ) ) ;
#1940 = LINE ( 'NONE', #5826, #14696 ) ;
#1941 = CARTESIAN_POINT ( 'NONE',  ( 37.69796330110505522, -0.5038408664219152788, 73.09843995877331224 ) ) ;
#1942 = ITEM_DEFINED_TRANSFORMATION ( 'NONE', 'NONE', #8430,  #2000 ) ;
#1943 = LINE ( 'NONE', #147, #23590 ) ;
#1944 = CARTESIAN_POINT ( 'NONE',  ( 37.69796330110504101, -21.11368208888610454, 69.66206559358661821 ) ) ;
#1945 = CIRCLE ( 'NONE', #24957, 1.750000000000001554 ) ;
#1946 = AXIS2_PLACEMENT_3D ( 'NONE', #15039, #5257, #19545 ) ;
#1947 = DIRECTION ( 'NONE',  ( 0.000000000000000000, 0.6568589528324746407, -0.7540134720837716742 ) ) ;
#1948 = EDGE_CURVE ( 'NONE', #8461, #10371, #20520, .T. ) ;
#1949 = CARTESIAN_POINT ( 'NONE',  ( 37.25202387243754032, -18.40384086642191974, 72.75271321436731853 ) ) ;
#1950 = CARTESIAN_POINT ( 'NONE',  ( 43.31606138205700063, -5.204193249396280585, 82.80501292736992980 ) ) ;
#1951 = CARTESIAN_POINT ( 'NONE',  ( 37.69796330110504101, -11.11368208888610276, 69.66206559358663242 ) ) ;
#1952 = ORIENTED_EDGE ( 'NONE', *, *, #16632, .F. ) ;
#1953 = CARTESIAN_POINT ( 'NONE',  ( 38.37017380507020192, -24.01368208888611022, 73.71602215082113219 ) ) ;
#1954 = VERTEX_POINT ( 'NONE', #22833 ) ;
#1955 = CARTESIAN_POINT ( 'NONE',  ( 40.06606138205700063, 5.594015759443068170, 2.006005027196319901 ) ) ;
#1956 = DIRECTION ( 'NONE',  ( -1.000000000000000000, -1.000000000000000078E-15, 0.000000000000000000 ) ) ;
#1957 = CARTESIAN_POINT ( 'NONE',  ( 38.37017380507018771, -25.60384086642191548, 70.24448340153875847 ) ) ;
#1958 = VERTEX_POINT ( 'NONE', #16654 ) ;
#1959 = VERTEX_POINT ( 'NONE', #23203 ) ;
#1960 = CYLINDRICAL_SURFACE ( 'NONE', #21172, 1.000000000000000888 ) ;
#1961 = CARTESIAN_POINT ( 'NONE',  ( 31.81606138205700418, 34.87886987267149408, 66.30501292737000085 ) ) ;
#1962 = CARTESIAN_POINT ( 'NONE',  ( 35.31606138205700773, 8.104266321858618838, 55.82104096753806033 ) ) ;
#1963 = CARTESIAN_POINT ( 'NONE',  ( 39.64521430340305841, -26.80384086642191832, 73.30173637941817333 ) ) ;
#1964 = AXIS2_PLACEMENT_3D ( 'NONE', #22242, #18267, #23913 ) ;
#1965 = CIRCLE ( 'NONE', #4849, 1.500000000000000222 ) ;
#1966 = AXIS2_PLACEMENT_3D ( 'NONE', #12340, #8340, #17621 ) ;
#1967 = SURFACE_STYLE_USAGE ( .BOTH. , #7915 ) ;
#1968 = CARTESIAN_POINT ( 'NONE',  ( 36.36258059203031934, -1.713682088886108179, 72.86986841596736042 ) ) ;
#1969 = CARTESIAN_POINT ( 'NONE',  ( 33.56606138205700773, 41.44123852234599070, 73.55501292736987295 ) ) ;
#1970 = ORIENTED_EDGE ( 'NONE', *, *, #10049, .F. ) ;
#1971 = VERTEX_POINT ( 'NONE', #3751 ) ;
#1972 = PLANE ( 'NONE',  #2191 ) ;
#1973 = LINE ( 'NONE', #9856, #22899 ) ;
#1974 = CARTESIAN_POINT ( 'NONE',  ( 37.80618814713138676, -23.70384086642190979, 69.62690120949091011 ) ) ;
#1975 =( NAMED_UNIT ( * ) PLANE_ANGLE_UNIT ( ) SI_UNIT ( $, .RADIAN. ) );
#1976 = DIRECTION ( 'NONE',  ( 1.000000000000000000, 2.751104698760144965E-15, -1.228345504986737969E-16 ) ) ;
#1977 = EDGE_LOOP ( 'NONE', ( #14482, #18335, #5715, #7299 ) ) ;
#1978 = DIRECTION ( 'NONE',  ( 2.341661252633485168E-15, -0.7516416929448815898, -0.6595716529892353686 ) ) ;
#1979 = EDGE_CURVE ( 'NONE', #2339, #23360, #5441, .T. ) ;
#1980 = DIRECTION ( 'NONE',  ( 0.000000000000000000, -3.469446951953611033E-15, -1.000000000000000000 ) ) ;
#1981 = DIRECTION ( 'NONE',  ( 1.000000000000000000, 0.000000000000000000, -0.000000000000000000 ) ) ;
#1982 = CARTESIAN_POINT ( 'NONE',  ( 38.37017380507018771, -3.603840866421911038, 70.24448340153877268 ) ) ;
#1983 = EDGE_LOOP ( 'NONE', ( #14043, #19238, #19687, #25097 ) ) ;
#1984 = TOROIDAL_SURFACE ( 'NONE', #17218, 1.000000000000000000, 1.000000000000000000 ) ;
#1985 = DIRECTION ( 'NONE',  ( -1.000000000000000000, -2.751104698760144965E-15, 1.228345504986737969E-16 ) ) ;
#1986 = VERTEX_POINT ( 'NONE', #25119 ) ;
#1987 = ORIENTED_EDGE ( 'NONE', *, *, #23271, .F. ) ;
#1988 = DIRECTION ( 'NONE',  ( -8.673617379884039170E-17, 1.163336342344335610E-15, -1.000000000000000000 ) ) ;
#1989 = CIRCLE ( 'NONE', #5293, 3.999999999999899636 ) ;
#1990 = CARTESIAN_POINT ( 'NONE',  ( 38.37017380507020192, -14.01368208888610312, 72.51602215082118619 ) ) ;
#1991 = VECTOR ( 'NONE', #3346, 1000.000000000000000 ) ;
#1992 = CARTESIAN_POINT ( 'NONE',  ( 37.38336156205274818, -11.71368208888610241, 72.12822762946750288 ) ) ;
#1993 = ORIENTED_EDGE ( 'NONE', *, *, #21629, .F. ) ;
#1994 = ORIENTED_EDGE ( 'NONE', *, *, #23549, .T. ) ;
#1995 = PLANE ( 'NONE',  #831 ) ;
#1996 = CARTESIAN_POINT ( 'NONE',  ( 38.31606138205700063, 15.19123852234700323, 70.30501292736995822 ) ) ;
#1997 = VERTEX_POINT ( 'NONE', #13310 ) ;
#1998 = DIRECTION ( 'NONE',  ( 0.000000000000000000, -2.999999999999999839E-15, -1.000000000000000000 ) ) ;
#1999 = CARTESIAN_POINT ( 'NONE',  ( 38.93415946300896024, -19.50384086642191050, 69.66206559358661821 ) ) ;
#2000 = AXIS2_PLACEMENT_3D ( 'NONE', #9286, #12766, #22537 ) ;
#2001 = EDGE_CURVE ( 'NONE', #5682, #24395, #7833, .T. ) ;
#2002 = EDGE_CURVE ( 'NONE', #18170, #19403, #7283, .T. ) ;
#2003 = CARTESIAN_POINT ( 'NONE',  ( 36.37840728046802496, -20.80772986314773831, 75.90997265879607880 ) ) ;
#2004 = DIRECTION ( 'NONE',  ( 1.000000000000000000, 0.000000000000000000, 0.000000000000000000 ) ) ;
#2005 = CARTESIAN_POINT ( 'NONE',  ( 37.89291511884476904, -19.11368208888609388, 70.26206559358661252 ) ) ;
#2006 = EDGE_CURVE ( 'NONE', #1520, #12430, #4412, .T. ) ;
#2007 = ORIENTED_EDGE ( 'NONE', *, *, #17291, .T. ) ;
#2008 = EDGE_CURVE ( 'NONE', #15541, #11322, #5825, .T. ) ;
#2009 = EDGE_CURVE ( 'NONE', #18901, #16151, #5224, .T. ) ;
#2010 = ORIENTED_EDGE ( 'NONE', *, *, #4137, .F. ) ;
#2011 = VECTOR ( 'NONE', #5994, 1000.000000000000000 ) ;
#2012 = CARTESIAN_POINT ( 'NONE',  ( 32.81606138205700773, 22.19123852234701388, 73.80501292736992980 ) ) ;
#2013 = CARTESIAN_POINT ( 'NONE',  ( 38.26194895904383486, -15.01368208888610134, 69.64448340153877837 ) ) ;
#2014 = LINE ( 'NONE', #25453, #14717 ) ;
#2015 = DIRECTION ( 'NONE',  ( -1.000000000000000000, 0.000000000000000000, 0.000000000000000000 ) ) ;
#2016 = AXIS2_PLACEMENT_3D ( 'NONE', #11059, #22397, #20344 ) ;
#2017 = CARTESIAN_POINT ( 'NONE',  ( 39.98359781491296161, -28.41368208888610525, 71.86517103874045631 ) ) ;
#2018 = DIRECTION ( 'NONE',  ( 1.000000000000000000, 1.734723475976805122E-16, -1.734723475976814737E-16 ) ) ;
#2019 = ADVANCED_FACE ( 'NONE', ( #11764 ), #19345, .F. ) ;
#2020 = ADVANCED_FACE ( 'NONE', ( #19218 ), #21279, .F. ) ;
#2021 = AXIS2_PLACEMENT_3D ( 'NONE', #13128, #4749, #12753 ) ;
#2022 = LINE ( 'NONE', #21993, #11513 ) ;
#2023 = ORIENTED_EDGE ( 'NONE', *, *, #19159, .F. ) ;
#2024 = CARTESIAN_POINT ( 'NONE',  ( 45.81606138205696510, -3.227578639999803212, -4.500312080287595329 ) ) ;
#2025 = ORIENTED_EDGE ( 'NONE', *, *, #18387, .T. ) ;
#2026 = VERTEX_POINT ( 'NONE', #3621 ) ;
#2027 = CARTESIAN_POINT ( 'NONE',  ( 39.12911128074872380, -5.503840866421911393, 69.06206559358666652 ) ) ;
#2028 = VECTOR ( 'NONE', #18443, 1000.000000000000000 ) ;
#2029 = ORIENTED_EDGE ( 'NONE', *, *, #24650, .F. ) ;
#2030 = CARTESIAN_POINT ( 'NONE',  ( 33.56606138205700773, 42.19123852234599070, 73.55501292736987295 ) ) ;
#2031 = CARTESIAN_POINT ( 'NONE',  ( 36.49096545463212493, -9.513682088886101340, 71.43714994484035685 ) ) ;
#2032 = VECTOR ( 'NONE', #13072, 1000.000000000000227 ) ;
#2033 = ORIENTED_EDGE ( 'NONE', *, *, #9098, .F. ) ;
#2034 = DIRECTION ( 'NONE',  ( -1.156482317317872465E-16, -0.4425581086832399702, 0.8967398287344626739 ) ) ;
#2035 = CARTESIAN_POINT ( 'NONE',  ( 29.81606138205697221, -3.984974717493133145, -3.847356352999882656 ) ) ;
#2036 = CARTESIAN_POINT ( 'NONE',  ( 36.29569395875879678, -13.31368208888610205, 69.98269868914867686 ) ) ;
#2037 = VECTOR ( 'NONE', #2768, 1000.000000000000000 ) ;
#2038 = EDGE_CURVE ( 'NONE', #7382, #23982, #19598, .T. ) ;
#2039 = CARTESIAN_POINT ( 'NONE',  ( 33.31606138205700773, -33.70281195181703993, 69.07320514641659770 ) ) ;
#2040 = DIRECTION ( 'NONE',  ( 0.000000000000000000, 1.000000000000000000, -3.469446951953613400E-15 ) ) ;
#2041 = AXIS2_PLACEMENT_3D ( 'NONE', #23198, #13678, #15348 ) ;
#2042 = DIRECTION ( 'NONE',  ( 0.000000000000000000, 3.469446951953613400E-15, 1.000000000000000000 ) ) ;
#2043 = VECTOR ( 'NONE', #9012, 1000.000000000000000 ) ;
#2044 = PLANE ( 'NONE',  #16388 ) ;
#2045 = CARTESIAN_POINT ( 'NONE',  ( 45.81606138205700063, -21.15876147765404625, 76.30501292736998664 ) ) ;
#2046 = AXIS2_PLACEMENT_3D ( 'NONE', #24848, #6964, #1149 ) ;
#2047 = CARTESIAN_POINT ( 'NONE',  ( 38.00113996487112189, -9.703840866421911571, 70.22690120949091863 ) ) ;
#2048 = CARTESIAN_POINT ( 'NONE',  ( 37.31647492878122563, -23.31368208888610383, 70.72433947564853440 ) ) ;
#2049 = ORIENTED_EDGE ( 'NONE', *, *, #4239, .T. ) ;
#2050 = CARTESIAN_POINT ( 'NONE',  ( 38.44690133353662276, -22.22127907754186893, 75.80501292736997243 ) ) ;
#2051 = DIRECTION ( 'NONE',  ( -2.048868001712896742E-15, 0.6595716529892345914, -0.7516416929448823669 ) ) ;
#2052 = ORIENTED_EDGE ( 'NONE', *, *, #22004, .F. ) ;
#2053 = ORIENTED_EDGE ( 'NONE', *, *, #3718, .F. ) ;
#2054 = EDGE_CURVE ( 'NONE', #16440, #19362, #7708, .T. ) ;
#2055 = VECTOR ( 'NONE', #19199, 1000.000000000000227 ) ;
#2056 = CARTESIAN_POINT ( 'NONE',  ( 37.50301148336529877, -26.50384086642192116, 73.69843995877326392 ) ) ;
#2057 = CARTESIAN_POINT ( 'NONE',  ( 39.41296390513587511, -24.41368208888610525, 71.67976084211548482 ) ) ;
#2058 = CARTESIAN_POINT ( 'NONE',  ( 40.55423172469004811, -4.413682088886105248, 72.05058123536544201 ) ) ;
#2059 = EDGE_LOOP ( 'NONE', ( #10504, #1303, #7748, #10759, #1267 ) ) ;
#2060 = PLANE ( 'NONE',  #11156 ) ;
#2061 = CARTESIAN_POINT ( 'NONE',  ( 39.02742774030101458, 0.5961591335780883627, 70.49320253461762320 ) ) ;
#2062 = EDGE_LOOP ( 'NONE', ( #19419, #10057, #1632, #10921 ) ) ;
#2063 = PLANE ( 'NONE',  #8048 ) ;
#2064 = CARTESIAN_POINT ( 'NONE',  ( 40.56606138205700773, 3.151453266960317023, 6.397347472316774031 ) ) ;
#2065 = CARTESIAN_POINT ( 'NONE',  ( 37.61123632939164452, -3.703840866421909794, 69.02690120949094421 ) ) ;
#2066 = DIRECTION ( 'NONE',  ( -1.000000000000000000, 0.000000000000000000, 0.000000000000000000 ) ) ;
#2067 = DIRECTION ( 'NONE',  ( -0.000000000000000000, -3.469446951953613400E-15, -1.000000000000000000 ) ) ;
#2068 = CARTESIAN_POINT ( 'NONE',  ( 40.14115730948191185, -16.51368208888610667, 71.32335560751960202 ) ) ;
#2069 = FACE_OUTER_BOUND ( 'NONE', #20298, .T. ) ;
#2070 = VECTOR ( 'NONE', #18574, 1000.000000000000000 ) ;
#2071 = CARTESIAN_POINT ( 'NONE',  ( 37.25202387243752611, -27.21368208888610241, 70.00779233799262613 ) ) ;
#2072 = VECTOR ( 'NONE', #5525, 1000.000000000000000 ) ;
#2073 = DIRECTION ( 'NONE',  ( 1.000000000000000000, 3.091505625455829092E-15, 4.515976121274730398E-17 ) ) ;
#2074 = CARTESIAN_POINT ( 'NONE',  ( 36.49096545463212493, -2.103840866421912370, 71.32335560751963044 ) ) ;
#2075 = DIRECTION ( 'NONE',  ( -1.000000000000000000, -2.827156040805656045E-15, 8.530177117963464484E-17 ) ) ;
#2076 = CARTESIAN_POINT ( 'NONE',  ( 37.69796330110504101, -17.11368208888610098, 69.66206559358661821 ) ) ;
#2077 = LINE ( 'NONE', #2210, #20968 ) ;
#2078 = ADVANCED_FACE ( 'NONE', ( #15477 ), #9448, .T. ) ;
#2079 = CARTESIAN_POINT ( 'NONE',  ( 36.64852494920107517, -20.20384086642191335, 71.86517103874048473 ) ) ;
#2080 = DIRECTION ( 'NONE',  ( 1.000000000000000000, 0.000000000000000000, 0.000000000000000000 ) ) ;
#2081 = EDGE_CURVE ( 'NONE', #22220, #12980, #20869, .T. ) ;
#2082 = CIRCLE ( 'NONE', #6616, 0.7500000000000006661 ) ;
#2083 = CARTESIAN_POINT ( 'NONE',  ( 39.38009889167650357, -14.21368208888610773, 72.75271321436731853 ) ) ;
#2084 = EDGE_LOOP ( 'NONE', ( #8923, #5906, #22734, #17854 ) ) ;
#2085 = CARTESIAN_POINT ( 'NONE',  ( 35.86008812008917346, -21.51368208888609956, 71.43714994484034264 ) ) ;
#2086 = EDGE_LOOP ( 'NONE', ( #18826, #3522, #1970, #2582 ) ) ;
#2087 = DIRECTION ( 'NONE',  ( 1.000000000000000275E-15, -0.9439899321577401858, -0.3299742535180970604 ) ) ;
#2088 = PLANE ( 'NONE',  #25150 ) ;
#2089 = AXIS2_PLACEMENT_3D ( 'NONE', #1604, #19524, #1985 ) ;
#2090 = CARTESIAN_POINT ( 'NONE',  ( 37.21915885897815457, -18.20384086642190979, 71.67976084211552745 ) ) ;
#2091 = ORIENTED_EDGE ( 'NONE', *, *, #12176, .F. ) ;
#2092 = ORIENTED_EDGE ( 'NONE', *, *, #11384, .F. ) ;
#2093 = DIRECTION ( 'NONE',  ( 0.000000000000000000, 2.999999999999999839E-15, 1.000000000000000000 ) ) ;
#2094 = DIRECTION ( 'NONE',  ( 0.000000000000000000, 0.000000000000000000, -1.000000000000000000 ) ) ;
#2095 = EDGE_LOOP ( 'NONE', ( #21744, #20124, #14575, #12917 ) ) ;
#2096 = CARTESIAN_POINT ( 'NONE',  ( 39.73277004305197124, -29.40384086642191264, 69.52238214136765748 ) ) ;
#2097 = CARTESIAN_POINT ( 'NONE',  ( 36.11133435605973574, 0.3863179111138967392, 72.15350918040385864 ) ) ;
#2098 = EDGE_CURVE ( 'NONE', #5909, #19241, #12645, .T. ) ;
#2099 = LINE ( 'NONE', #23861, #23765 ) ;
#2100 = VERTEX_POINT ( 'NONE', #21035 ) ;
#2101 = VERTEX_POINT ( 'NONE', #25378 ) ;
#2102 = CARTESIAN_POINT ( 'NONE',  ( 36.10895460087045450, 5.484131741160450879, 69.30501292736998664 ) ) ;
#2103 = CARTESIAN_POINT ( 'NONE',  ( 44.81606138205700063, -34.67340937580780036, 71.26505871168839690 ) ) ;
#2104 = CARTESIAN_POINT ( 'NONE',  ( 36.87297107704151244, -19.90384086642190553, 70.26145752964255564 ) ) ;
#2105 = DIRECTION ( 'NONE',  ( -1.000000000000000000, -1.000000000000000078E-15, 0.000000000000000000 ) ) ;
#2106 = COLOUR_RGB ( '', 0.40784314, 0.44705882, 0.49803922) ;
#2107 = EDGE_LOOP ( 'NONE', ( #4877, #14552, #7560, #24954, #3602, #24123 ) ) ;
#2108 = DIRECTION ( 'NONE',  ( 1.000000000000000000, 0.000000000000000000, 0.000000000000000000 ) ) ;
#2109 = MECHANICAL_DESIGN_GEOMETRIC_PRESENTATION_REPRESENTATION (  '', ( #21879 ), #6646 ) ;
#2110 = DIRECTION ( 'NONE',  ( 0.000000000000000000, -0.5706330172266913525, 0.8212051873014213355 ) ) ;
#2111 = EDGE_LOOP ( 'NONE', ( #21458, #24071, #20598, #8543 ) ) ;
#2112 = CARTESIAN_POINT ( 'NONE',  ( 37.31647492878124694, -8.303840866421912992, 72.03616607671141026 ) ) ;
#2113 = LINE ( 'NONE', #24002, #23315 ) ;
#2114 = EDGE_LOOP ( 'NONE', ( #1105, #6601, #14755, #24647 ) ) ;
#2115 = DIRECTION ( 'NONE',  ( 1.209079903702923825E-31, -1.000000000000000000, 3.325260651745651169E-15 ) ) ;
#2116 = ORIENTED_EDGE ( 'NONE', *, *, #7384, .F. ) ;
#2117 = VERTEX_POINT ( 'NONE', #3376 ) ;
#2118 = DIRECTION ( 'NONE',  ( -1.000000000000000000, 0.000000000000000000, 0.000000000000000000 ) ) ;
#2119 = CARTESIAN_POINT ( 'NONE',  ( 38.93987200065208754, -2.813682088886101162, 70.42958956619168021 ) ) ;
#2120 = CARTESIAN_POINT ( 'NONE',  ( 38.00113996487114321, -3.913682088886100807, 72.53360434286905445 ) ) ;
#2121 = ORIENTED_EDGE ( 'NONE', *, *, #3983, .T. ) ;
#2122 = EDGE_LOOP ( 'NONE', ( #4301, #13864, #16625, #3133 ) ) ;
#2123 = FACE_OUTER_BOUND ( 'NONE', #15305, .T. ) ;
#2124 = DIRECTION ( 'NONE',  ( 1.000000000000000000, 0.000000000000000000, -0.000000000000000000 ) ) ;
#2125 = EDGE_LOOP ( 'NONE', ( #16708, #15029, #1457, #1398 ) ) ;
#2126 = DIRECTION ( 'NONE',  ( 1.156482317317872711E-16, 0.4425581086832400257, -0.8967398287344628960 ) ) ;
#2127 = CARTESIAN_POINT ( 'NONE',  ( 38.93415946300896024, -15.50384086642190873, 69.66206559358661821 ) ) ;
#2128 = VECTOR ( 'NONE', #7850, 1000.000000000000000 ) ;
#2129 = CARTESIAN_POINT ( 'NONE',  ( 36.80559154321147020, -21.57317817398384108, 75.83174599736526034 ) ) ;
#2130 = ADVANCED_FACE ( 'NONE', ( #15603 ), #23459, .F. ) ;
#2131 = VECTOR ( 'NONE', #1486, 1000.000000000000227 ) ;
#2132 = CARTESIAN_POINT ( 'NONE',  ( 33.31606138205700773, -14.32738121993777192, 11.12118157620986558 ) ) ;
#2133 = CARTESIAN_POINT ( 'NONE',  ( 39.51027997493896748, -20.51368208888610312, 71.32335560751960202 ) ) ;
#2134 = VERTEX_POINT ( 'NONE', #17170 ) ;
#2135 = ORIENTED_EDGE ( 'NONE', *, *, #6726, .F. ) ;
#2136 = DIRECTION ( 'NONE',  ( 0.000000000000000000, -0.5706330172266919076, 0.8212051873014208914 ) ) ;
#2137 = CARTESIAN_POINT ( 'NONE',  ( 37.25202387243752611, -13.21368208888610063, 70.00779233799262613 ) ) ;
#2138 = LINE ( 'NONE', #18006, #20063 ) ;
#2139 = DIRECTION ( 'NONE',  ( -1.000000000000000000, -1.187136597504755470E-16, -8.249087426255173666E-17 ) ) ;
#2140 = DIRECTION ( 'NONE',  ( -1.000000000000000000, 6.018531076210130433E-31, 1.734723475976804876E-16 ) ) ;
#2141 = FACE_OUTER_BOUND ( 'NONE', #11810, .T. ) ;
#2142 = VECTOR ( 'NONE', #25060, 1000.000000000000000 ) ;
#2143 = LINE ( 'NONE', #6156, #6973 ) ;
#2144 = DIRECTION ( 'NONE',  ( -2.312964634635742267E-15, 0.8967398287344634511, 0.4425581086832385824 ) ) ;
#2145 = ADVANCED_FACE ( 'NONE', ( #24993 ), #7380, .T. ) ;
#2146 = ORIENTED_EDGE ( 'NONE', *, *, #8766, .T. ) ;
#2147 = EDGE_CURVE ( 'NONE', #21524, #17894, #4402, .T. ) ;
#2148 = AXIS2_PLACEMENT_3D ( 'NONE', #23261, #1613, #5622 ) ;
#2149 = CARTESIAN_POINT ( 'NONE',  ( 36.98894827842408262, -21.72323602677954923, 75.31699084059582106 ) ) ;
#2150 = ORIENTED_EDGE ( 'NONE', *, *, #4100, .F. ) ;
#2151 = EDGE_CURVE ( 'NONE', #23532, #22006, #19727, .T. ) ;
#2152 = EDGE_LOOP ( 'NONE', ( #3581, #6754, #7192, #10219 ) ) ;
#2153 = CARTESIAN_POINT ( 'NONE',  ( 37.61123632939164452, -3.703840866421909794, 69.02690120949094421 ) ) ;
#2154 = EDGE_CURVE ( 'NONE', #3400, #23482, #8135, .T. ) ;
#2155 = EDGE_CURVE ( 'NONE', #25416, #8151, #22591, .T. ) ;
#2156 = VERTEX_POINT ( 'NONE', #9482 ) ;
#2157 = VECTOR ( 'NONE', #20748, 1000.000000000000000 ) ;
#2158 = FACE_OUTER_BOUND ( 'NONE', #8481, .T. ) ;
#2159 = CARTESIAN_POINT ( 'NONE',  ( 36.68196826583682935, -7.613682088886103649, 71.96809898377890136 ) ) ;
#2160 = VECTOR ( 'NONE', #13117, 1000.000000000000000 ) ;
#2161 = ORIENTED_EDGE ( 'NONE', *, *, #22066, .T. ) ;
#2162 = CARTESIAN_POINT ( 'NONE',  ( 44.81606138205700063, -11.72563467517899838, 72.98595903681223263 ) ) ;
#2163 = ADVANCED_FACE ( 'NONE', ( #19632 ), #15390, .F. ) ;
#2164 = CARTESIAN_POINT ( 'NONE',  ( 36.89935272106204422, -15.21368208888610063, 69.52238214136768590 ) ) ;
#2165 = AXIS2_PLACEMENT_3D ( 'NONE', #15015, #24281, #9111 ) ;
#2166 = CARTESIAN_POINT ( 'NONE',  ( 42.99362197529018914, 2.839053354292388143, 6.102835146812753742 ) ) ;
#2167 = DIRECTION ( 'NONE',  ( 1.000000000000000000, 2.999999999999999839E-15, 0.000000000000000000 ) ) ;
#2168 = VECTOR ( 'NONE', #22569, 1000.000000000000114 ) ;
#2169 = DIRECTION ( 'NONE',  ( -8.758115402030106693E-47, 1.000000000000000000, -3.469446951953613400E-15 ) ) ;
#2170 = SURFACE_STYLE_USAGE ( .BOTH. , #11599 ) ;
#2171 = LINE ( 'NONE', #15953, #13139 ) ;
#2172 = VECTOR ( 'NONE', #15012, 1000.000000000000000 ) ;
#2173 = CARTESIAN_POINT ( 'NONE',  ( 43.81606138205700063, 8.191238522346990791, 65.80501292736998664 ) ) ;
#2174 = CARTESIAN_POINT ( 'NONE',  ( 38.31606138205700063, -29.78523130861184143, 52.92072663988442116 ) ) ;
#2175 = CARTESIAN_POINT ( 'NONE',  ( 39.24876120206128860, -24.71368208888610241, 70.63227792289242757 ) ) ;
#2176 = ORIENTED_EDGE ( 'NONE', *, *, #11481, .F. ) ;
#2177 = CARTESIAN_POINT ( 'NONE',  ( 40.31606138205700063, 8.691238522346997897, 68.80501292736998664 ) ) ;
#2178 = VECTOR ( 'NONE', #12286, 1000.000000000000227 ) ;
#2179 = DIRECTION ( 'NONE',  ( 3.469446951953614189E-15, -0.8967398287344635621, -0.4425581086832386379 ) ) ;
#2180 = EDGE_LOOP ( 'NONE', ( #1763, #24910, #20575, #23053 ) ) ;
#2181 = ORIENTED_EDGE ( 'NONE', *, *, #18945, .F. ) ;
#2182 = AXIS2_PLACEMENT_3D ( 'NONE', #14350, #551, #47 ) ;
#2183 = CARTESIAN_POINT ( 'NONE',  ( 40.52078840805429394, -25.00384086642191761, 72.15350918040381600 ) ) ;
#2184 = EDGE_CURVE ( 'NONE', #4421, #25070, #3535, .T. ) ;
#2185 = AXIS2_PLACEMENT_3D ( 'NONE', #8014, #22033, #15852 ) ;
#2186 = CARTESIAN_POINT ( 'NONE',  ( 36.49096545463212493, -27.51368208888610312, 71.43714994484030001 ) ) ;
#2187 = CARTESIAN_POINT ( 'NONE',  ( 33.31606138205700773, 3.043703737701412226, 64.67489359404071081 ) ) ;
#2188 = CARTESIAN_POINT ( 'NONE',  ( 39.31564783533279694, -1.303840866421910105, 70.72433947564853440 ) ) ;
#2189 = DIRECTION ( 'NONE',  ( 0.000000000000000000, 1.000000000000000000, -2.775557561562891351E-15 ) ) ;
#2190 = VERTEX_POINT ( 'NONE', #25289 ) ;
#2191 = AXIS2_PLACEMENT_3D ( 'NONE', #5859, #11796, #547 ) ;
#2192 = CARTESIAN_POINT ( 'NONE',  ( 33.40064408022072939, 42.57231754924293909, 79.37823623207320622 ) ) ;
#2193 = DIRECTION ( 'NONE',  ( -1.000000000000000000, 0.000000000000000000, 0.000000000000000000 ) ) ;
#2194 = EDGE_CURVE ( 'NONE', #8063, #11585, #13719, .T. ) ;
#2195 = CARTESIAN_POINT ( 'NONE',  ( 40.52078840805429394, -1.003840866421915612, 72.15350918040385864 ) ) ;
#2196 = CARTESIAN_POINT ( 'NONE',  ( 38.31606138205700063, -1.054793099133682244, 61.76760556592023477 ) ) ;
#2197 = DIRECTION ( 'NONE',  ( 0.000000000000000000, 2.999999999999999839E-15, 1.000000000000000000 ) ) ;
#2198 = CARTESIAN_POINT ( 'NONE',  ( 39.75915168707250302, -6.713682088886099741, 70.26145752964252722 ) ) ;
#2199 = DIRECTION ( 'NONE',  ( -1.000000000000000000, 5.204170427930413997E-31, 1.734723475976804876E-16 ) ) ;
#2200 = CARTESIAN_POINT ( 'NONE',  ( 36.64852494920107517, -25.41368208888610525, 70.89533451361945993 ) ) ;
#2201 = AXIS2_PLACEMENT_3D ( 'NONE', #24335, #14817, #6707 ) ;
#2202 = CARTESIAN_POINT ( 'NONE',  ( 44.81606138205700063, 40.39281886181299797, 81.44836866983821722 ) ) ;
#2203 = EDGE_CURVE ( 'NONE', #154, #2408, #9356, .T. ) ;
#2204 = AXIS2_PLACEMENT_3D ( 'NONE', #3710, #15442, #24951 ) ;
#2205 = CARTESIAN_POINT ( 'NONE',  ( 39.95015449827720744, -5.003840866421912281, 71.96809898377888715 ) ) ;
#2206 = B_SPLINE_CURVE_WITH_KNOTS ( 'NONE', 3,
 ( #8105, #15951, #2539, #6429, #4246, #10424 ),
 .UNSPECIFIED., .F., .F.,
 ( 4, 2, 4 ),
 ( 0.000000000000000000, 0.5000000000000000000, 1.000000000000000000 ),
 .UNSPECIFIED. ) ;
#2207 = CARTESIAN_POINT ( 'NONE',  ( 43.21596744901363962, 3.650325757544471195, 6.335220020744675828 ) ) ;
#2208 = CARTESIAN_POINT ( 'NONE',  ( 38.73920764526923932, -27.50384086642191406, 70.26206559358661252 ) ) ;
#2209 = CARTESIAN_POINT ( 'NONE',  ( 36.68196826583682935, -9.613682088886104538, 71.96809898377890136 ) ) ;
#2210 = CARTESIAN_POINT ( 'NONE',  ( 30.81606138205705037, -30.65246816789535345, 72.44500581826353880 ) ) ;
#2211 = CARTESIAN_POINT ( 'NONE',  ( 38.82593461698265003, -12.70384086642191512, 73.13360434286903455 ) ) ;
#2212 = LINE ( 'NONE', #16120, #11823 ) ;
#2213 = CARTESIAN_POINT ( 'NONE',  ( 36.49096545463212493, -9.513682088886101340, 71.43714994484035685 ) ) ;
#2214 = VERTEX_POINT ( 'NONE', #13842 ) ;
#2215 = CARTESIAN_POINT ( 'NONE',  ( 39.02088643472237095, -16.91368208888609814, 69.02690120949091579 ) ) ;
#2216 = VERTEX_POINT ( 'NONE', #5988 ) ;
#2217 = CARTESIAN_POINT ( 'NONE',  ( 40.52316816324353965, 5.484131741160450879, 69.30501292736998664 ) ) ;
#2218 = VECTOR ( 'NONE', #11281, 1000.000000000000227 ) ;
#2219 = CIRCLE ( 'NONE', #23197, 1.500000000000001332 ) ;
#2220 = LINE ( 'NONE', #15877, #21515 ) ;
#2221 = CARTESIAN_POINT ( 'NONE',  ( 38.26194895904384197, -18.60384086642190837, 72.51602215082118619 ) ) ;
#2222 = ORIENTED_EDGE ( 'NONE', *, *, #20103, .F. ) ;
#2223 = ORIENTED_EDGE ( 'NONE', *, *, #11008, .T. ) ;
#2224 = LINE ( 'NONE', #4423, #8434 ) ;
#2225 = AXIS2_PLACEMENT_3D ( 'NONE', #3016, #16941, #7154 ) ;
#2226 = DIRECTION ( 'NONE',  ( 0.000000000000000000, 0.7540134720837717852, 0.6568589528324746407 ) ) ;
#2227 = CARTESIAN_POINT ( 'NONE',  ( 36.11133435605973574, -20.00384086642191406, 70.60699637195608602 ) ) ;
#2228 = PLANE ( 'NONE',  #24849 ) ;
#2229 = CARTESIAN_POINT ( 'NONE',  ( 36.64852494920107517, -25.41368208888610525, 70.89533451361945993 ) ) ;
#2230 = CARTESIAN_POINT ( 'NONE',  ( 44.81606138205700063, -31.45856502260510013, 77.07494475056050476 ) ) ;
#2231 = EDGE_CURVE ( 'NONE', #3938, #16606, #1973, .T. ) ;
#2232 = VERTEX_POINT ( 'NONE', #4048 ) ;
#2233 = EDGE_CURVE ( 'NONE', #24557, #120, #7668, .T. ) ;
#2234 = CARTESIAN_POINT ( 'NONE',  ( 40.31606138205699352, -9.274586591516573719, 29.12776117315710067 ) ) ;
#2235 = PRODUCT_DEFINITION_FORMATION_WITH_SPECIFIED_SOURCE ( 'ANY', '', #3964, .NOT_KNOWN. ) ;
#2236 = CARTESIAN_POINT ( 'NONE',  ( 32.81606138205700773, -24.55876147765401285, 70.30501292737008612 ) ) ;
#2237 = CARTESIAN_POINT ( 'NONE',  ( 39.98359781491296161, -23.20384086642191335, 70.89533451361945993 ) ) ;
#2238 = VECTOR ( 'NONE', #2346, 1000.000000000000000 ) ;
#2239 = PLANE ( 'NONE',  #7123 ) ;
#2240 = ORIENTED_EDGE ( 'NONE', *, *, #6083, .T. ) ;
#2241 = FACE_OUTER_BOUND ( 'NONE', #11521, .T. ) ;
#2242 = DIRECTION ( 'NONE',  ( 0.000000000000000000, -0.6568589528324746407, 0.7540134720837717852 ) ) ;
#2243 = CARTESIAN_POINT ( 'NONE',  ( 38.93987200065210175, -0.8038408664219099942, 72.33091598616827866 ) ) ;
#2244 = DIRECTION ( 'NONE',  ( 0.6571615412467028960, -0.6189832172005511612, -0.4301145028132777881 ) ) ;
#2245 = VERTEX_POINT ( 'NONE', #19762 ) ;
#2246 = EDGE_CURVE ( 'NONE', #4432, #8461, #1928, .T. ) ;
#2247 = DIRECTION ( 'NONE',  ( 0.000000000000000000, 0.3299742535180922864, -0.9439899321577417401 ) ) ;
#2248 = ORIENTED_EDGE ( 'NONE', *, *, #17169, .F. ) ;
#2249 = EDGE_LOOP ( 'NONE', ( #3554, #6520, #9600, #21223 ) ) ;
#2250 = CARTESIAN_POINT ( 'NONE',  ( 38.31606138205700773, -21.82678658219787948, 29.70634659473178019 ) ) ;
#2251 = CARTESIAN_POINT ( 'NONE',  ( 28.81606138205696155, 0.8576245772853319238, -1.570935883000529332 ) ) ;
#2252 = CARTESIAN_POINT ( 'NONE',  ( 37.21915885897815457, -7.413682088886101695, 71.08074471024443142 ) ) ;
#2253 = CARTESIAN_POINT ( 'NONE',  ( 37.69225076346193504, -3.813682088886102051, 72.33091598616827866 ) ) ;
#2254 = VERTEX_POINT ( 'NONE', #19254 ) ;
#2255 = EDGE_LOOP ( 'NONE', ( #4585, #7218, #14724, #219 ) ) ;
#2256 = DIRECTION ( 'NONE',  ( 1.000000000000000000, 2.168404344971010101E-16, -1.734723475976814737E-16 ) ) ;
#2257 = DIRECTION ( 'NONE',  ( -1.067465804653198538E-15, 0.4425581086832399147, -0.8967398287344627850 ) ) ;
#2258 = ORIENTED_EDGE ( 'NONE', *, *, #6571, .F. ) ;
#2259 = DIRECTION ( 'NONE',  ( -1.000000000000000000, 0.000000000000000000, 0.000000000000000000 ) ) ;
#2260 = CARTESIAN_POINT ( 'NONE',  ( 39.29254315202757653, -8.803840866421912992, 72.81632618279323310 ) ) ;
#2261 = DIRECTION ( 'NONE',  ( 1.000000000000000000, 0.000000000000000000, 0.000000000000000000 ) ) ;
#2262 = LINE ( 'NONE', #10389, #24934 ) ;
#2263 = ORIENTED_EDGE ( 'NONE', *, *, #23409, .T. ) ;
#2264 = ORIENTED_EDGE ( 'NONE', *, *, #12872, .T. ) ;
#2265 = CARTESIAN_POINT ( 'NONE',  ( 33.31606138205700773, 3.099306811489555891, 65.29760936252343129 ) ) ;
#2266 = CARTESIAN_POINT ( 'NONE',  ( 39.38009889167650357, -10.21368208888610773, 72.75271321436733274 ) ) ;
#2267 = CARTESIAN_POINT ( 'NONE',  ( 32.81606138205700773, 2.740850673309605412, 6.112030963703427133 ) ) ;
#2268 = FACE_OUTER_BOUND ( 'NONE', #23283, .T. ) ;
#2269 = DIRECTION ( 'NONE',  ( 0.000000000000000000, 1.000000000000000000, -3.304235192336775512E-15 ) ) ;
#2270 = PLANE ( 'NONE',  #24587 ) ;
#2271 = AXIS2_PLACEMENT_3D ( 'NONE', #630, #4518, #19980 ) ;
#2272 = DIRECTION ( 'NONE',  ( 0.000000000000000000, -2.999999999999999839E-15, -1.000000000000000000 ) ) ;
#2273 = CARTESIAN_POINT ( 'NONE',  ( 36.31606138205700063, -31.05876147765400574, 73.55501292737010033 ) ) ;
#2274 = VERTEX_POINT ( 'NONE', #23112 ) ;
#2275 = EDGE_CURVE ( 'NONE', #18597, #10242, #17586, .T. ) ;
#2276 = CARTESIAN_POINT ( 'NONE',  ( 37.48451232389217580, -22.04143432302674555, 75.30659729247206258 ) ) ;
#2277 = EDGE_LOOP ( 'NONE', ( #12064, #434, #20219 ) ) ;
#2278 = EDGE_LOOP ( 'NONE', ( #13540, #2635, #12420, #15880 ) ) ;
#2279 = CARTESIAN_POINT ( 'NONE',  ( 36.81465384343994884, 42.57231754924293909, 79.57823623207322328 ) ) ;
#2280 = CARTESIAN_POINT ( 'NONE',  ( 36.11133435605973574, -2.003840866421913169, 70.60699637195612866 ) ) ;
#2281 = ORIENTED_EDGE ( 'NONE', *, *, #15480, .T. ) ;
#2282 = DIRECTION ( 'NONE',  ( 1.734723475976804876E-16, 3.491481338843135327E-15, 1.000000000000000000 ) ) ;
#2283 = CARTESIAN_POINT ( 'NONE',  ( 38.26194895904383486, -9.013682088886101340, 69.64448340153879258 ) ) ;
#2284 = ORIENTED_EDGE ( 'NONE', *, *, #890, .T. ) ;
#2285 = LINE ( 'NONE', #98, #3817 ) ;
#2286 = CARTESIAN_POINT ( 'NONE',  ( 37.50301148336529167, -15.11368208888610098, 69.06206559358665231 ) ) ;
#2287 = DIRECTION ( 'NONE',  ( -1.000000000000000000, -2.930207641762116835E-15, -1.414177847953724077E-16 ) ) ;
#2288 = PLANE ( 'NONE',  #19857 ) ;
#2289 = ADVANCED_FACE ( 'NONE', ( #15510 ), #13347, .T. ) ;
#2290 = VERTEX_POINT ( 'NONE', #11411 ) ;
#2291 = DIRECTION ( 'NONE',  ( -1.734723475976804876E-16, -3.552713678800500140E-15, -1.000000000000000000 ) ) ;
#2292 = ADVANCED_FACE ( 'NONE', ( #1715 ), #3926, .F. ) ;
#2293 = SURFACE_STYLE_FILL_AREA ( #20953 ) ;
#2294 = LINE ( 'NONE', #14284, #22983 ) ;
#2295 = LINE ( 'NONE', #5926, #23610 ) ;
#2296 = DIRECTION ( 'NONE',  ( 1.000000000000000000, -0.000000000000000000, -0.000000000000000000 ) ) ;
#2297 = CARTESIAN_POINT ( 'NONE',  ( 39.02742774030102879, -26.21368208888610241, 72.26730301774232146 ) ) ;
#2298 = EDGE_LOOP ( 'NONE', ( #9215, #19456, #10247, #6097 ) ) ;
#2299 = CARTESIAN_POINT ( 'NONE',  ( 38.96215273200666473, -22.12375471166958008, 75.80539210339577494 ) ) ;
#2300 = EDGE_CURVE ( 'NONE', #1142, #13410, #11797, .T. ) ;
#2301 = DIRECTION ( 'NONE',  ( -3.083952846180990083E-15, 1.000000000000000000, -2.999999999999998655E-15 ) ) ;
#2302 = VERTEX_POINT ( 'NONE', #23240 ) ;
#2303 = ORIENTED_EDGE ( 'NONE', *, *, #25191, .T. ) ;
#2304 = CARTESIAN_POINT ( 'NONE',  ( 35.86008812008917346, -22.10384086642191548, 71.32335560751961623 ) ) ;
#2305 = PRODUCT ( 'Leaf Spring', 'Leaf Spring', '', ( #24242 ) ) ;
#2306 = CARTESIAN_POINT ( 'NONE',  ( 39.98359781491296161, -26.41368208888610525, 71.86517103874045631 ) ) ;
#2307 = DIRECTION ( 'NONE',  ( 1.000000000000000000, 0.000000000000000000, 0.000000000000000000 ) ) ;
#2308 = PLANE ( 'NONE',  #16359 ) ;
#2309 = VERTEX_POINT ( 'NONE', #5602 ) ;
#2310 = DIRECTION ( 'NONE',  ( 1.836970198721029688E-16, 2.999999999999999839E-15, 1.000000000000000000 ) ) ;
#2311 = CARTESIAN_POINT ( 'NONE',  ( 43.31606138205700063, 2.715274261285174351, 65.05190033008260286 ) ) ;
#2312 = CARTESIAN_POINT ( 'NONE',  ( 36.11133435605973574, -2.003840866421913169, 70.60699637195612866 ) ) ;
#2313 = ADVANCED_FACE ( 'NONE', ( #5860 ), #25412, .F. ) ;
#2314 = LINE ( 'NONE', #8131, #13998 ) ;
#2315 = DIRECTION ( 'NONE',  ( 0.000000000000000000, 1.000000000000000000, -2.999999999999999839E-15 ) ) ;
#2316 = CARTESIAN_POINT ( 'NONE',  ( 39.29254315202756231, -6.813682088886101162, 69.94417936956673998 ) ) ;
#2317 = CARTESIAN_POINT ( 'NONE',  ( 36.31606138205699352, 8.691238522346996120, 69.09790614618343341 ) ) ;
#2318 = ADVANCED_FACE ( 'NONE', ( #13594 ), #21444, .T. ) ;
#2319 = CARTESIAN_POINT ( 'NONE',  ( 38.37017380507020192, -24.01368208888610667, 73.11602215082115208 ) ) ;
#2320 = EDGE_CURVE ( 'NONE', #23734, #16934, #7796, .T. ) ;
#2321 = EDGE_CURVE ( 'NONE', #13207, #3634, #2356, .T. ) ;
#2322 = EDGE_CURVE ( 'NONE', #6643, #22414, #10576, .T. ) ;
#2323 = CARTESIAN_POINT ( 'NONE',  ( 36.81606138205700063, 6.191238522346988127, 65.30501292736998664 ) ) ;
#2324 = CARTESIAN_POINT ( 'NONE',  ( 39.98359781491296161, -5.203840866421911571, 70.89533451361947414 ) ) ;
#2325 = CONTEXT_DEPENDENT_SHAPE_REPRESENTATION ( #5202, #4388 ) ;
#2326 = DIRECTION ( 'NONE',  ( 1.000000000000000000, 1.000000000000000078E-15, 0.000000000000000000 ) ) ;
#2327 = CARTESIAN_POINT ( 'NONE',  ( 39.31564783533279694, -23.30384086642191477, 70.72433947564853440 ) ) ;
#2328 = CARTESIAN_POINT ( 'NONE',  ( 36.68196826583682935, -13.61368208888610454, 71.96809898377888715 ) ) ;
#2329 = LINE ( 'NONE', #392, #6554 ) ;
#2330 = ADVANCED_FACE ( 'NONE', ( #18466 ), #12564, .T. ) ;
#2331 = AXIS2_PLACEMENT_3D ( 'NONE', #17338, #25419, #5366 ) ;
#2332 = CARTESIAN_POINT ( 'NONE',  ( 39.29254315202757653, -10.80384086642191477, 72.81632618279323310 ) ) ;
#2333 = DIRECTION ( 'NONE',  ( 0.000000000000000000, 1.000000000000000000, -2.999999999999999839E-15 ) ) ;
#2334 = AXIS2_PLACEMENT_3D ( 'NONE', #7760, #17297, #7500 ) ;
#2335 = VECTOR ( 'NONE', #4912, 1000.000000000000114 ) ;
#2336 = CARTESIAN_POINT ( 'NONE',  ( 38.82593461698262871, -10.91368208888609992, 69.62690120949091011 ) ) ;
#2337 = EDGE_LOOP ( 'NONE', ( #22884, #21057, #12205, #7070 ) ) ;
#2338 = CARTESIAN_POINT ( 'NONE',  ( 37.50301148336529167, -17.11368208888609743, 69.06206559358665231 ) ) ;
#2339 = VERTEX_POINT ( 'NONE', #4565 ) ;
#2340 = DIRECTION ( 'NONE',  ( 1.734723475976804876E-16, 3.491481338843135327E-15, 1.000000000000000000 ) ) ;
#2341 = CARTESIAN_POINT ( 'NONE',  ( 46.81606138205697221, -4.349482454670835274, -5.142398479549302515 ) ) ;
#2342 = CARTESIAN_POINT ( 'NONE',  ( 37.89291511884479036, -16.50384086642191050, 72.49843995877330372 ) ) ;
#2343 = ORIENTED_EDGE ( 'NONE', *, *, #13920, .T. ) ;
#2344 = ADVANCED_FACE ( 'NONE', ( #6238 ), #22329, .F. ) ;
#2345 = VERTEX_POINT ( 'NONE', #16392 ) ;
#2346 = DIRECTION ( 'NONE',  ( -0.000000000000000000, -0.000000000000000000, -1.000000000000000000 ) ) ;
#2347 = DIRECTION ( 'NONE',  ( 1.734723475976804876E-16, 3.469446951953610245E-15, 1.000000000000000000 ) ) ;
#2348 = CARTESIAN_POINT ( 'NONE',  ( 40.52078840805429394, -25.00384086642191761, 72.15350918040381600 ) ) ;
#2349 = CARTESIAN_POINT ( 'NONE',  ( 33.31606138205700773, -26.06829118875200635, 72.80501292736998664 ) ) ;
#2350 = CARTESIAN_POINT ( 'NONE',  ( 39.82603832034400426, -28.31368208888610027, 72.40698646996131060 ) ) ;
#2351 = CARTESIAN_POINT ( 'NONE',  ( 43.81606138205700063, 0.9984178969752143251, 11.59873562314662010 ) ) ;
#2352 = CIRCLE ( 'NONE', #12251, 1.000000000000000888 ) ;
#2353 = VERTEX_POINT ( 'NONE', #10618 ) ;
#2354 = CIRCLE ( 'NONE', #14697, 12.59999999999999964 ) ;
#2355 = CARTESIAN_POINT ( 'NONE',  ( 33.63430211860926278, 2.841683824787794688, 6.101742829876990015 ) ) ;
#2356 = LINE ( 'NONE', #4314, #3984 ) ;
#2357 = CARTESIAN_POINT ( 'NONE',  ( 38.82593461698264292, -18.70384086642191690, 73.13360434286903455 ) ) ;
#2358 =( LENGTH_UNIT ( ) NAMED_UNIT ( * ) SI_UNIT ( .MILLI., .METRE. ) );
#2359 = DIRECTION ( 'NONE',  ( 1.000000000000000000, -3.083952846180990083E-15, 9.251858538542970050E-30 ) ) ;
#2360 = ORIENTED_EDGE ( 'NONE', *, *, #4498, .F. ) ;
#2361 = FACE_OUTER_BOUND ( 'NONE', #20310, .T. ) ;
#2362 = FACE_OUTER_BOUND ( 'NONE', #8970, .T. ) ;
#2363 = CARTESIAN_POINT ( 'NONE',  ( 40.14115730948191185, -29.10384086642190482, 71.43714994484028580 ) ) ;
#2364 = FACE_OUTER_BOUND ( 'NONE', #2249, .T. ) ;
#2365 = ORIENTED_EDGE ( 'NONE', *, *, #10064, .T. ) ;
#2366 = CARTESIAN_POINT ( 'NONE',  ( 43.31606138205700063, 7.043113989679085307, 66.83274420321491505 ) ) ;
#2367 = VERTEX_POINT ( 'NONE', #18099 ) ;
#2368 = ORIENTED_EDGE ( 'NONE', *, *, #21667, .F. ) ;
#2369 = AXIS2_PLACEMENT_3D ( 'NONE', #14550, #4758, #9023 ) ;
#2370 = CARTESIAN_POINT ( 'NONE',  ( 43.31606138205695089, 3.741517323833267294, 2.753690589366190711 ) ) ;
#2372 = EDGE_CURVE ( 'NONE', #24574, #9515, #15507, .T. ) ;
#2371 = DIRECTION ( 'NONE',  ( -9.027796614315171564E-31, -1.000000000000000000, -3.938893903907230117E-15 ) ) ;
#2373 = CARTESIAN_POINT ( 'NONE',  ( 39.02742774030102879, -6.213682088886101518, 72.26730301774236409 ) ) ;
#2374 = EDGE_CURVE ( 'NONE', #14477, #15409, #8051, .T. ) ;
#2375 = VECTOR ( 'NONE', #15926, 1000.000000000000000 ) ;
#2376 = CARTESIAN_POINT ( 'NONE',  ( 37.31647492878122563, -7.313682088886101162, 70.72433947564853440 ) ) ;
#2377 = ORIENTED_EDGE ( 'NONE', *, *, #11194, .F. ) ;
#2378 = PRODUCT_RELATED_PRODUCT_CATEGORY ( 'part', '', ( #1662 ) ) ;
#2379 = EDGE_LOOP ( 'NONE', ( #2999, #17890, #19541, #15459 ) ) ;
#2380 = DIRECTION ( 'NONE',  ( -8.758115402030106693E-47, 1.000000000000000000, -3.469446951953613400E-15 ) ) ;
#2381 = LINE ( 'NONE', #4202, #9181 ) ;
#2382 = ORIENTED_EDGE ( 'NONE', *, *, #25220, .F. ) ;
#2383 = CARTESIAN_POINT ( 'NONE',  ( 43.81606138205700063, -33.00876147765401925, 70.30501292737011454 ) ) ;
#2384 = CARTESIAN_POINT ( 'NONE',  ( 36.49096545463212493, -12.10384086642191193, 71.32335560751961623 ) ) ;
#2385 = DIRECTION ( 'NONE',  ( 0.000000000000000000, 0.000000000000000000, 1.000000000000000000 ) ) ;
#2386 = CARTESIAN_POINT ( 'NONE',  ( 31.56606138205697576, -5.022037326221730602, -5.474317061061731771 ) ) ;
#2387 = ORIENTED_EDGE ( 'NONE', *, *, #23881, .F. ) ;
#2388 = VERTEX_POINT ( 'NONE', #8301 ) ;
#2389 = ORIENTED_EDGE ( 'NONE', *, *, #12473, .F. ) ;
#2390 = CARTESIAN_POINT ( 'NONE',  ( 30.81606138205700418, 40.34464305740947054, 81.44836866983821722 ) ) ;
#2391 = CARTESIAN_POINT ( 'NONE',  ( 37.69796330110504101, -9.113682088886100985, 69.66206559358664663 ) ) ;
#2392 = ADVANCED_FACE ( 'NONE', ( #10112 ), #20018, .T. ) ;
#2393 = CARTESIAN_POINT ( 'NONE',  ( 40.31606138205700773, -31.05876147765399864, 75.30501292737008612 ) ) ;
#2394 = DIRECTION ( 'NONE',  ( 1.000000000000000000, 0.000000000000000000, 0.000000000000000000 ) ) ;
#2395 = AXIS2_PLACEMENT_3D ( 'NONE', #14635, #3156, #12719 ) ;
#2396 = DIRECTION ( 'NONE',  ( 0.000000000000000000, 1.000000000000000000, 0.000000000000000000 ) ) ;
#2397 = PLANE ( 'NONE',  #13514 ) ;
#2398 = LINE ( 'NONE', #19807, #6565 ) ;
#2399 = DIRECTION ( 'NONE',  ( -4.625929269271484533E-15, 0.8967398287344634511, 0.4425581086832385824 ) ) ;
#2400 = CARTESIAN_POINT ( 'NONE',  ( 30.81606138205697931, -5.918777154956195830, -5.916875169744970187 ) ) ;
#2401 = VERTEX_POINT ( 'NONE', #417 ) ;
#2402 = EDGE_LOOP ( 'NONE', ( #20983, #1543, #25185, #10638 ) ) ;
#2404 = EDGE_CURVE ( 'NONE', #6235, #17478, #14094, .T. ) ;
#2403 = CARTESIAN_POINT ( 'NONE',  ( 44.31606138205700063, 10.62769494289597993, 68.29765714199933768 ) ) ;
#2405 = CARTESIAN_POINT ( 'NONE',  ( 36.11133435605973574, -4.003840866421914946, 70.60699637195612866 ) ) ;
#2406 = PRESENTATION_LAYER_ASSIGNMENT (  '', '', ( #8604 ) ) ;
#2407 = EDGE_CURVE ( 'NONE', #12138, #13165, #17997, .T. ) ;
#2408 = VERTEX_POINT ( 'NONE', #14228 ) ;
#2409 = DIRECTION ( 'NONE',  ( 0.000000000000000000, -0.6568589528324746407, 0.7540134720837717852 ) ) ;
#2410 = CARTESIAN_POINT ( 'NONE',  ( 38.37017380507020192, -10.01368208888611022, 73.11602215082118050 ) ) ;
#2411 = COLOUR_RGB ( '', 0.66274510, 0.83137255, 0.94901961) ;
#2412 = CIRCLE ( 'NONE', #16825, 1.000000000000000888 ) ;
#2413 = CARTESIAN_POINT ( 'NONE',  ( 38.53272007700518742, 38.19123852234600491, 72.53609335118615320 ) ) ;
#2414 = CARTESIAN_POINT ( 'NONE',  ( 39.73277004305198545, -16.21368208888610596, 73.23812341099225875 ) ) ;
#2415 = CIRCLE ( 'NONE', #11489, 1.250000000000000888 ) ;
#2416 = DIRECTION ( 'NONE',  ( -9.027796614315171564E-31, -1.000000000000000000, -3.938893903907230117E-15 ) ) ;
#2417 = LINE ( 'NONE', #10295, #3390 ) ;
#2418 = ADVANCED_FACE ( 'NONE', ( #15891 ), #6372, .F. ) ;
#2419 = CARTESIAN_POINT ( 'NONE',  ( 38.31606138205700063, -30.30876147765401996, 69.30501292737010033 ) ) ;
#2420 = CIRCLE ( 'NONE', #20143, 1.500000000000001332 ) ;
#2421 = LINE ( 'NONE', #8239, #8598 ) ;
#2422 = CARTESIAN_POINT ( 'NONE',  ( 30.81606138205700418, -38.55876147765410167, 70.30501292737011454 ) ) ;
#2423 = FACE_OUTER_BOUND ( 'NONE', #7251, .T. ) ;
#2424 = CARTESIAN_POINT ( 'NONE',  ( 38.37017380507020192, -26.01368208888610312, 72.51602215082114355 ) ) ;
#2425 = AXIS2_PLACEMENT_3D ( 'NONE', #11642, #15614, #23466 ) ;
#2426 = EDGE_LOOP ( 'NONE', ( #3479, #7297, #23375, #11174 ) ) ;
#2427 = FACE_OUTER_BOUND ( 'NONE', #23941, .T. ) ;
#2428 = CARTESIAN_POINT ( 'NONE',  ( 31.81606138205700418, -24.55876147765401996, 67.80501292737008612 ) ) ;
#2429 = ORIENTED_EDGE ( 'NONE', *, *, #14200, .T. ) ;
#2430 = ORIENTED_EDGE ( 'NONE', *, *, #20190, .F. ) ;
#2431 = CARTESIAN_POINT ( 'NONE',  ( 40.33642880535521869, -21.30384086642190766, 69.98269868914866265 ) ) ;
#2432 = CIRCLE ( 'NONE', #5738, 2.000000000000001776 ) ;
#2433 = CARTESIAN_POINT ( 'NONE',  ( 39.75915168707250302, -24.71368208888610241, 70.26145752964249880 ) ) ;
#2434 = DIRECTION ( 'NONE',  ( -1.000000000000000000, 1.301042606982604506E-30, 4.336808689942015271E-16 ) ) ;
#2435 = AXIS2_PLACEMENT_3D ( 'NONE', #23279, #13502, #23400 ) ;
#2436 = VECTOR ( 'NONE', #18030, 1000.000000000000000 ) ;
#2437 = CARTESIAN_POINT ( 'NONE',  ( 43.31606138205700063, -12.87480755223282358, 20.78922580900563588 ) ) ;
#2438 = ORIENTED_EDGE ( 'NONE', *, *, #9873, .T. ) ;
#2439 = CARTESIAN_POINT ( 'NONE',  ( 38.57646292309977554, -5.204259650130242498, 82.80501292736988717 ) ) ;
#2440 = CARTESIAN_POINT ( 'NONE',  ( 33.31606138205700773, -20.93319939328399926, 43.78741072286599945 ) ) ;
#2441 = CARTESIAN_POINT ( 'NONE',  ( 36.36258059203030513, -3.903840866421911748, 69.89063713639259845 ) ) ;
#2442 = PLANE ( 'NONE',  #3297 ) ;
#2443 = AXIS2_PLACEMENT_3D ( 'NONE', #4060, #8182, #10241 ) ;
#2444 = FACE_OUTER_BOUND ( 'NONE', #15215, .T. ) ;
#2445 = CARTESIAN_POINT ( 'NONE',  ( 39.38009889167650357, -6.213682088886108623, 72.75271321436733274 ) ) ;
#2446 = CARTESIAN_POINT ( 'NONE',  ( 35.52536905565747105, -37.40916500673439771, 83.30501292737011454 ) ) ;
#2447 = CARTESIAN_POINT ( 'NONE',  ( 39.98359781491296161, -28.41368208888610525, 71.86517103874045631 ) ) ;
#2448 = CIRCLE ( 'NONE', #20155, 1.750000000000001554 ) ;
#2449 = CARTESIAN_POINT ( 'NONE',  ( 40.31606138205697221, -2.780187754385547105, -4.367921789353634843 ) ) ;
#2450 = CARTESIAN_POINT ( 'NONE',  ( 40.56606138205696510, -1.522470315718718270, 0.9921758631592225708 ) ) ;
#2451 = CARTESIAN_POINT ( 'NONE',  ( 37.38336156205273397, -23.90384086642191619, 70.63227792289245599 ) ) ;
#2452 = CARTESIAN_POINT ( 'NONE',  ( 36.87297107704152666, -11.71368208888611129, 72.49904802271740323 ) ) ;
#2453 = FACE_OUTER_BOUND ( 'NONE', #3327, .T. ) ;
#2454 = CIRCLE ( 'NONE', #11126, 1.800000000000002931 ) ;
#2455 = CARTESIAN_POINT ( 'NONE',  ( 37.69796330110505522, -10.50384086642190873, 73.09843995877331224 ) ) ;
#2456 = DIRECTION ( 'NONE',  ( 0.000000000000000000, 0.4425581086832397482, -0.8967398287344626739 ) ) ;
#2457 = EDGE_CURVE ( 'NONE', #8692, #22403, #21950, .T. ) ;
#2458 = CARTESIAN_POINT ( 'NONE',  ( 40.14115730948191185, -10.51368208888609956, 71.32335560751961623 ) ) ;
#2459 = EDGE_LOOP ( 'NONE', ( #2389, #9279, #960, #1890 ) ) ;
#2460 = PRODUCT_DEFINITION_SHAPE ( 'NONE', 'NONE',  #25501 ) ;
#2461 = CARTESIAN_POINT ( 'NONE',  ( 40.77203464402485622, -14.51368208888610312, 71.32335560751960202 ) ) ;
#2462 = ORIENTED_EDGE ( 'NONE', *, *, #10200, .T. ) ;
#2463 = CARTESIAN_POINT ( 'NONE',  ( 31.81606138205700418, -21.15876147765404625, 76.30501292736998664 ) ) ;
#2464 = ADVANCED_FACE ( 'NONE', ( #8174 ), #670, .F. ) ;
#2465 = DIRECTION ( 'NONE',  ( -0.1733269559585509378, 0.000000000000000000, -0.9848643390529188135 ) ) ;
#2466 = CARTESIAN_POINT ( 'NONE',  ( 39.37952058850012804, -19.00384086642191406, 71.78268878715390144 ) ) ;
#2467 = EDGE_CURVE ( 'NONE', #14211, #17608, #8557, .T. ) ;
#2468 = EDGE_CURVE ( 'NONE', #9599, #12562, #16016, .T. ) ;
#2469 = VERTEX_POINT ( 'NONE', #20147 ) ;
#2470 = CIRCLE ( 'NONE', #5777, 3.000000000000002665 ) ;
#2471 = ORIENTED_EDGE ( 'NONE', *, *, #8526, .F. ) ;
#2472 = FACE_OUTER_BOUND ( 'NONE', #17154, .T. ) ;
#2473 = DIRECTION ( 'NONE',  ( -1.000000000000000000, -2.168404344971060144E-16, 1.734723475976814737E-16 ) ) ;
#2474 = CARTESIAN_POINT ( 'NONE',  ( 39.73277004305197124, -23.40384086642191264, 69.52238214136768590 ) ) ;
#2475 = VECTOR ( 'NONE', #10305, 1000.000000000000000 ) ;
#2476 = CARTESIAN_POINT ( 'NONE',  ( 32.81606138205700773, 45.92314894770293421, 79.37823623207320622 ) ) ;
#2477 = CARTESIAN_POINT ( 'NONE',  ( 38.37017380507020192, -28.01368208888610667, 73.11602215082115208 ) ) ;
#2478 = ADVANCED_FACE ( 'NONE', ( #2483 ), #10355, .F. ) ;
#2479 = CARTESIAN_POINT ( 'NONE',  ( 31.81606138205700418, -21.15876147765410309, 66.30501292737000085 ) ) ;
#2480 = ADVANCED_FACE ( 'NONE', ( #8934 ), #25385, .F. ) ;
#2481 = ORIENTED_EDGE ( 'NONE', *, *, #12234, .F. ) ;
#2482 = CARTESIAN_POINT ( 'NONE',  ( 36.31606138205700063, -4.357181138186127178, 82.80501292736992980 ) ) ;
#2483 = FACE_OUTER_BOUND ( 'NONE', #24444, .T. ) ;
#2484 = CARTESIAN_POINT ( 'NONE',  ( 37.25202387243754032, -12.40384086642191619, 72.75271321436731853 ) ) ;
#2485 = DIRECTION ( 'NONE',  ( -3.083952846180990083E-15, -1.000000000000000000, 2.999999999999999839E-15 ) ) ;
#2486 = VECTOR ( 'NONE', #242, 1000.000000000000227 ) ;
#2487 = FACE_OUTER_BOUND ( 'NONE', #14398, .T. ) ;
#2488 = ADVANCED_FACE ( 'NONE', ( #24748 ), #9075, .T. ) ;
#2489 = AXIS2_PLACEMENT_3D ( 'NONE', #19390, #23374, #13359 ) ;
#2490 = DIRECTION ( 'NONE',  ( 0.000000000000000000, 1.000000000000000000, -3.469446951953614189E-15 ) ) ;
#2491 = CARTESIAN_POINT ( 'NONE',  ( 38.63098279924290068, 1.296159133578087763, 72.53360434286905445 ) ) ;
#2492 = LINE ( 'NONE', #16276, #13869 ) ;
#2493 = ORIENTED_EDGE ( 'NONE', *, *, #20622, .F. ) ;
#2494 = DIRECTION ( 'NONE',  ( -1.786044098272412642E-16, -0.4425581086832399702, 0.8967398287344628960 ) ) ;
#2495 = ORIENTED_EDGE ( 'NONE', *, *, #14029, .T. ) ;
#2496 = VERTEX_POINT ( 'NONE', #24614 ) ;
#2497 = LINE ( 'NONE', #6759, #16866 ) ;
#2498 = CARTESIAN_POINT ( 'NONE',  ( 43.31606138205700063, 6.699978067258562042, 7.424159817622362212 ) ) ;
#2499 = UNCERTAINTY_MEASURE_WITH_UNIT (LENGTH_MEASURE( 1.000000000000000082E-05 ), #2755, 'distance_accuracy_value', 'NONE');
#2500 = CARTESIAN_POINT ( 'NONE',  ( 39.24876120206128860, -6.713682088886101518, 70.63227792289247020 ) ) ;
#2501 = CARTESIAN_POINT ( 'NONE',  ( 37.60469502381300089, -7.213682088886102406, 70.49320253461759478 ) ) ;
#2502 = ORIENTED_EDGE ( 'NONE', *, *, #12738, .T. ) ;
#2503 = VERTEX_POINT ( 'NONE', #10991 ) ;
#2504 = LINE ( 'NONE', #16287, #25087 ) ;
#2505 = CARTESIAN_POINT ( 'NONE',  ( 36.06606138205700063, 6.004618353093779781, 2.291321535809666354 ) ) ;
#2506 = ORIENTED_EDGE ( 'NONE', *, *, #7660, .T. ) ;
#2507 = CARTESIAN_POINT ( 'NONE',  ( 40.06606138205700063, 5.719301844480432884, 2.701924129460374413 ) ) ;
#2508 = CARTESIAN_POINT ( 'NONE',  ( 36.64852494920107517, -10.20384086642191157, 71.86517103874049894 ) ) ;
#2509 = DIRECTION ( 'NONE',  ( 1.514188661106530005E-31, 1.000000000000000000, -2.999999999999999839E-15 ) ) ;
#2510 = DIRECTION ( 'NONE',  ( 0.000000000000000000, -2.999999999999999839E-15, -1.000000000000000000 ) ) ;
#2511 = ORIENTED_EDGE ( 'NONE', *, *, #19188, .T. ) ;
#2512 = ORIENTED_EDGE ( 'NONE', *, *, #4337, .T. ) ;
#2513 = EDGE_LOOP ( 'NONE', ( #25331, #17268, #5891, #10881 ) ) ;
#2514 = LINE ( 'NONE', #14380, #3833 ) ;
#2515 = CARTESIAN_POINT ( 'NONE',  ( 37.80618814713140097, -7.913682088886108801, 73.13360434286904876 ) ) ;
#2516 = LINE ( 'NONE', #10397, #8144 ) ;
#2517 = LINE ( 'NONE', #6151, #23965 ) ;
#2518 = CARTESIAN_POINT ( 'NONE',  ( 38.82593461698262871, -26.91368208888610170, 69.62690120949091011 ) ) ;
#2519 = PLANE ( 'NONE',  #1559 ) ;
#2520 = EDGE_CURVE ( 'NONE', #16389, #15899, #14302, .T. ) ;
#2521 = EDGE_CURVE ( 'NONE', #3225, #11274, #11125, .T. ) ;
#2522 = CARTESIAN_POINT ( 'NONE',  ( 45.81606138205700063, -31.45856502260500065, 77.07494475056050476 ) ) ;
#2523 = CARTESIAN_POINT ( 'NONE',  ( 33.66606138205698073, -6.672912525257930660, -0.4345143786932820218 ) ) ;
#2524 = LINE ( 'NONE', #466, #7852 ) ;
#2525 = VERTEX_POINT ( 'NONE', #7126 ) ;
#2526 = ORIENTED_EDGE ( 'NONE', *, *, #9282, .T. ) ;
#2527 = VECTOR ( 'NONE', #7330, 1000.000000000000000 ) ;
#2528 = FACE_OUTER_BOUND ( 'NONE', #778, .T. ) ;
#2529 = CARTESIAN_POINT ( 'NONE',  ( 36.89935272106205133, -4.403840866421918854, 73.23812341099225875 ) ) ;
#2530 = CARTESIAN_POINT ( 'NONE',  ( 37.31647492878122563, -21.31368208888610027, 70.72433947564853440 ) ) ;
#2531 = VERTEX_POINT ( 'NONE', #5197 ) ;
#2532 = VERTEX_POINT ( 'NONE', #24368 ) ;
#2533 = CIRCLE ( 'NONE', #21472, 0.2000000000000057288 ) ;
#2534 = LINE ( 'NONE', #606, #24325 ) ;
#2535 = CARTESIAN_POINT ( 'NONE',  ( 38.26194895904383486, -7.013682088886100452, 69.64448340153879258 ) ) ;
#2536 = PLANE ( 'NONE',  #20690 ) ;
#2537 = CARTESIAN_POINT ( 'NONE',  ( 40.55423172469004811, -14.41368208888610347, 72.05058123536544201 ) ) ;
#2538 = CARTESIAN_POINT ( 'NONE',  ( 36.31606138205700773, -23.16691978223482096, 31.29201591705069063 ) ) ;
#2539 = CARTESIAN_POINT ( 'NONE',  ( 32.85323118609061055, 3.754743573466610140, 6.231177976620426051 ) ) ;
#2540 = AXIS2_PLACEMENT_3D ( 'NONE', #22311, #11074, #21118 ) ;
#2541 = EDGE_CURVE ( 'NONE', #16347, #15938, #6745, .T. ) ;
#2542 = CARTESIAN_POINT ( 'NONE',  ( 39.64305411916487287, -29.01274100871117767, 69.84207103023153707 ) ) ;
#2543 = APPLICATION_CONTEXT ( 'automotive_design' ) ;
#2544 = ADVANCED_FACE ( 'NONE', ( #13055 ), #14719, .F. ) ;
#2545 = CARTESIAN_POINT ( 'NONE',  ( 43.31606138205700063, -13.04008168869994222, 21.66778101221729713 ) ) ;
#2546 = ADVANCED_FACE ( 'NONE', ( #14982 ), #22579, .F. ) ;
#2547 = VECTOR ( 'NONE', #4398, 1000.000000000000227 ) ;
#2548 = FACE_OUTER_BOUND ( 'NONE', #14715, .T. ) ;
#2549 = CYLINDRICAL_SURFACE ( 'NONE', #13146, 0.7500000000000006661 ) ;
#2550 = CARTESIAN_POINT ( 'NONE',  ( 37.21915885897815457, -23.41368208888610170, 71.08074471024441721 ) ) ;
#2551 = VERTEX_POINT ( 'NONE', #6996 ) ;
#2552 = CARTESIAN_POINT ( 'NONE',  ( 39.20536636138601949, -22.01741677639897077, 75.30191219513037026 ) ) ;
#2553 = AXIS2_PLACEMENT_3D ( 'NONE', #228, #14278, #21886 ) ;
#2554 = CARTESIAN_POINT ( 'NONE',  ( 33.31606138205700773, 10.06218483883314718, 67.80501292737497465 ) ) ;
#2555 = ORIENTED_EDGE ( 'NONE', *, *, #9425, .T. ) ;
#2556 = ORIENTED_EDGE ( 'NONE', *, *, #24059, .F. ) ;
#2557 = CARTESIAN_POINT ( 'NONE',  ( 39.64521430340305841, -26.80384086642191832, 73.30173637941817333 ) ) ;
#2558 = ADVANCED_FACE ( 'NONE', ( #17049 ), #14846, .F. ) ;
#2559 = CARTESIAN_POINT ( 'NONE',  ( 38.37017380507020192, -28.01368208888610667, 73.11602215082115208 ) ) ;
#2560 = DIRECTION ( 'NONE',  ( -1.000000000000000000, 1.115179377413661005E-30, 3.717264591378870232E-16 ) ) ;
#2561 = AXIS2_PLACEMENT_3D ( 'NONE', #3982, #21505, #3856 ) ;
#2562 = CARTESIAN_POINT ( 'NONE',  ( 43.31606138205700063, -37.98241563432385703, 69.85268917996594951 ) ) ;
#2563 = DIRECTION ( 'NONE',  ( 1.000000000000000000, 0.000000000000000000, 0.000000000000000000 ) ) ;
#2564 = VERTEX_POINT ( 'NONE', #5323 ) ;
#2565 = CARTESIAN_POINT ( 'NONE',  ( 44.06606138205700063, 43.35512946304240245, 82.37823623207322044 ) ) ;
#2566 = CARTESIAN_POINT ( 'NONE',  ( 45.81606138205707168, -38.42645682328033985, 63.90656833300437256 ) ) ;
#2567 = AXIS2_PLACEMENT_3D ( 'NONE', #21845, #11433, #2257 ) ;
#2568 = CARTESIAN_POINT ( 'NONE',  ( 36.36258059203030513, -1.903840866421910638, 69.89063713639259845 ) ) ;
#2569 = CARTESIAN_POINT ( 'NONE',  ( 41.31606138205700063, 7.282926244446937147, 65.60596383066929604 ) ) ;
#2570 = CARTESIAN_POINT ( 'NONE',  ( 39.82603832034400426, -8.313682088886110932, 72.40698646996135324 ) ) ;
#2571 = FACE_OUTER_BOUND ( 'NONE', #4228, .T. ) ;
#2572 = VECTOR ( 'NONE', #586, 1000.000000000000227 ) ;
#2573 = AXIS2_PLACEMENT_3D ( 'NONE', #16977, #2914, #7188 ) ;
#2574 = CARTESIAN_POINT ( 'NONE',  ( 36.80608444377001121, -25.31368208888610383, 70.35351908239857721 ) ) ;
#2575 = DIRECTION ( 'NONE',  ( -1.000000000000000000, -1.734723475976804876E-16, 1.734723475976814737E-16 ) ) ;
#2576 = AXIS2_PLACEMENT_3D ( 'NONE', #3929, #9485, #9616 ) ;
#2577 = DIRECTION ( 'NONE',  ( 1.000000000000000000, 0.000000000000000000, -0.000000000000000000 ) ) ;
#2578 = CARTESIAN_POINT ( 'NONE',  ( 37.69225076346193504, -25.80384086642191477, 70.42958956619166599 ) ) ;
#2579 = CARTESIAN_POINT ( 'NONE',  ( 37.25202387243752611, -11.21368208888610241, 70.00779233799262613 ) ) ;
#2580 = CARTESIAN_POINT ( 'NONE',  ( 43.31606138205700063, -27.25871422114667553, 59.79942265548595515 ) ) ;
#2581 = AXIS2_PLACEMENT_3D ( 'NONE', #8423, #2473, #21813 ) ;
#2582 = ORIENTED_EDGE ( 'NONE', *, *, #4044, .F. ) ;
#2583 = CARTESIAN_POINT ( 'NONE',  ( 36.80608444377001831, -12.30384086642191299, 72.40698646996135324 ) ) ;
#2584 = CARTESIAN_POINT ( 'NONE',  ( 32.81606138205700773, -40.62725863591898445, 68.52362519861142687 ) ) ;
#2585 = CIRCLE ( 'NONE', #16172, 0.5000000000000005551 ) ;
#2586 = EDGE_CURVE ( 'NONE', #13895, #14345, #1185, .T. ) ;
#2587 = CARTESIAN_POINT ( 'NONE',  ( 36.87297107704152666, -3.713682088886109511, 72.49904802271743165 ) ) ;
#2588 = ORIENTED_EDGE ( 'NONE', *, *, #25480, .T. ) ;
#2589 = CARTESIAN_POINT ( 'NONE',  ( 40.77203464402485622, -16.51368208888610667, 71.32335560751960202 ) ) ;
#2590 = VERTEX_POINT ( 'NONE', #5067 ) ;
#2591 = PLANE ( 'NONE',  #21386 ) ;
#2592 = CARTESIAN_POINT ( 'NONE',  ( 33.31606138205700773, 9.733755362416909307, 68.18201966341686671 ) ) ;
#2593 = CARTESIAN_POINT ( 'NONE',  ( 38.93987200065210175, -20.80384086642191122, 72.33091598616826445 ) ) ;
#2594 = ORIENTED_EDGE ( 'NONE', *, *, #5792, .F. ) ;
#2595 = VERTEX_POINT ( 'NONE', #18723 ) ;
#2596 = CARTESIAN_POINT ( 'NONE',  ( 43.31606138205700063, -22.22127907754187959, 75.30501292736998664 ) ) ;
#2597 = DIRECTION ( 'NONE',  ( 0.000000000000000000, -1.000000000000000000, 2.999999999999999839E-15 ) ) ;
#2598 = CARTESIAN_POINT ( 'NONE',  ( 39.02088643472237806, -22.70384086642191690, 73.73360434286898624 ) ) ;
#2599 = CIRCLE ( 'NONE', #7965, 0.2000000000000057288 ) ;
#2600 = CARTESIAN_POINT ( 'NONE',  ( 43.81608638205700146, 2.761903742731119049, 12.21527246050395377 ) ) ;
#2601 = CARTESIAN_POINT ( 'NONE',  ( 39.38009889167650357, -26.21368208888610951, 72.75271321436730432 ) ) ;
#2602 = DIRECTION ( 'NONE',  ( 0.000000000000000000, -1.000000000000000000, 3.469446951953701358E-15 ) ) ;
#2603 = AXIS2_PLACEMENT_3D ( 'NONE', #7492, #5819, #11370 ) ;
#2604 = FACE_OUTER_BOUND ( 'NONE', #7979, .T. ) ;
#2605 = ADVANCED_FACE ( 'NONE', ( #2988 ), #7254, .T. ) ;
#2606 = EDGE_LOOP ( 'NONE', ( #14663, #13840, #20351 ) ) ;
#2607 = CARTESIAN_POINT ( 'NONE',  ( 31.81606138205700418, -26.74044063519535186, 82.55501292737007191 ) ) ;
#2608 = EDGE_CURVE ( 'NONE', #9423, #562, #927, .T. ) ;
#2609 = CARTESIAN_POINT ( 'NONE',  ( 33.31606138205700773, -22.22127907754180853, 85.30501292736998664 ) ) ;
#2610 = CARTESIAN_POINT ( 'NONE',  ( 39.75915168707251723, -16.90384086642191619, 72.49904802271738902 ) ) ;
#2611 = EDGE_CURVE ( 'NONE', #23726, #17894, #3379, .T. ) ;
#2612 = DIRECTION ( 'NONE',  ( 0.000000000000000000, 0.000000000000000000, 1.000000000000000000 ) ) ;
#2613 = DIRECTION ( 'NONE',  ( -1.156482317317870739E-16, -0.4425581086832400257, 0.8967398287344628960 ) ) ;
#2614 = ADVANCED_FACE ( 'NONE', ( #12934 ), #22453, .F. ) ;
#2615 =( GEOMETRIC_REPRESENTATION_CONTEXT ( 3 ) GLOBAL_UNCERTAINTY_ASSIGNED_CONTEXT ( ( #18541 ) ) GLOBAL_UNIT_ASSIGNED_CONTEXT ( ( #13905, #21761, #17912 ) ) REPRESENTATION_CONTEXT ( 'NONE', 'WORKASPACE' ) );
#2616 = DIRECTION ( 'NONE',  ( 1.000000000000000000, 0.000000000000000000, 0.000000000000000000 ) ) ;
#2617 = VECTOR ( 'NONE', #17651, 1000.000000000000000 ) ;
#2618 = CARTESIAN_POINT ( 'NONE',  ( 3.816061382056946449, 1.361611432489073570, -2.592146606185760316 ) ) ;
#2619 = CARTESIAN_POINT ( 'NONE',  ( 37.12184278917507640, -2.103840866421912370, 71.32335560751961623 ) ) ;
#2620 = FACE_OUTER_BOUND ( 'NONE', #14305, .T. ) ;
#2621 = ORIENTED_EDGE ( 'NONE', *, *, #5162, .T. ) ;
#2622 = VECTOR ( 'NONE', #19427, 1000.000000000000000 ) ;
#2623 = EDGE_CURVE ( 'NONE', #18307, #12298, #15934, .T. ) ;
#2624 = CARTESIAN_POINT ( 'NONE',  ( 38.26194895904383486, -25.01368208888610312, 69.64448340153876416 ) ) ;
#2625 = VERTEX_POINT ( 'NONE', #23461 ) ;
#2626 = ORIENTED_EDGE ( 'NONE', *, *, #22495, .F. ) ;
#2627 = CARTESIAN_POINT ( 'NONE',  ( 36.31606138205699352, 8.691238522346985462, 65.51211970855652567 ) ) ;
#2628 = LINE ( 'NONE', #2743, #6750 ) ;
#2629 = CARTESIAN_POINT ( 'NONE',  ( 37.38336156205274818, -3.713682088886102406, 72.12822762946751709 ) ) ;
#2630 = CARTESIAN_POINT ( 'NONE',  ( 38.00113996487114321, -5.913682088886099919, 72.53360434286905445 ) ) ;
#2631 = VERTEX_POINT ( 'NONE', #9328 ) ;
#2632 = EDGE_LOOP ( 'NONE', ( #5538, #17725, #314, #8172 ) ) ;
#2633 = DIRECTION ( 'NONE',  ( 0.000000000000000000, -0.6568589528324746407, 0.7540134720837717852 ) ) ;
#2634 = CARTESIAN_POINT ( 'NONE',  ( 40.31606138205701484, -21.83924545618510393, 28.60179643084731893 ) ) ;
#2635 = ORIENTED_EDGE ( 'NONE', *, *, #25431, .F. ) ;
#2636 = CARTESIAN_POINT ( 'NONE',  ( 38.37017380507018771, -11.60384086642190660, 69.64448340153879258 ) ) ;
#2637 = CARTESIAN_POINT ( 'NONE',  ( 34.81606138205700773, -14.36460986495925241, 36.24727600202827915 ) ) ;
#2638 = MECHANICAL_DESIGN_GEOMETRIC_PRESENTATION_REPRESENTATION (  '', ( #21575 ), #8410 ) ;
#2639 = DIRECTION ( 'NONE',  ( 1.000000000000000000, 0.000000000000000000, 0.000000000000000000 ) ) ;
#2640 = EDGE_LOOP ( 'NONE', ( #20648, #25357, #18740, #12834 ) ) ;
#2641 = VECTOR ( 'NONE', #11145, 1000.000000000000000 ) ;
#2642 = EDGE_LOOP ( 'NONE', ( #4611, #1847, #18235, #21818 ) ) ;
#2643 = ORIENTED_EDGE ( 'NONE', *, *, #23871, .T. ) ;
#2644 = FACE_OUTER_BOUND ( 'NONE', #7408, .T. ) ;
#2645 = CARTESIAN_POINT ( 'NONE',  ( 36.68196826583682935, -5.613682088886105426, 71.96809898377890136 ) ) ;
#2646 = VECTOR ( 'NONE', #9349, 1000.000000000000114 ) ;
#2647 = DIRECTION ( 'NONE',  ( 0.000000000000000000, -0.8191520442889929088, -0.5735764363510444941 ) ) ;
#2648 = CARTESIAN_POINT ( 'NONE',  ( 35.64099152588522657, 0.3928188618129990761, 73.02501292736999972 ) ) ;
#2649 = ADVANCED_FACE ( 'NONE', ( #17680 ), #17299, .F. ) ;
#2650 = EDGE_CURVE ( 'NONE', #3066, #7328, #17172, .T. ) ;
#2651 = CARTESIAN_POINT ( 'NONE',  ( 43.38751061443460344, 3.099069811988895751, 6.135932541694130826 ) ) ;
#2652 = CARTESIAN_POINT ( 'NONE',  ( 36.31606138205700063, 9.191238522346999673, 69.30501292736997243 ) ) ;
#2653 = CARTESIAN_POINT ( 'NONE',  ( 32.81606138205700773, 22.19123852234699967, 69.30501292736994401 ) ) ;
#2654 = EDGE_CURVE ( 'NONE', #23852, #1577, #8534, .T. ) ;
#2655 = CARTESIAN_POINT ( 'NONE',  ( 36.31606138205702905, -20.48366339139476011, 75.45349498244979713 ) ) ;
#2656 = ORIENTED_EDGE ( 'NONE', *, *, #17591, .T. ) ;
#2657 = ORIENTED_EDGE ( 'NONE', *, *, #14433, .F. ) ;
#2658 = DIRECTION ( 'NONE',  ( 1.218693434051482139E-16, -0.4425581086832393041, 0.8967398287344630070 ) ) ;
#2659 = CARTESIAN_POINT ( 'NONE',  ( 40.33642880535524000, -28.31368208888611093, 72.77780686321125359 ) ) ;
#2660 = CARTESIAN_POINT ( 'NONE',  ( 38.73920764526925353, -24.11368208888610098, 72.49843995877328950 ) ) ;
#2661 = EDGE_LOOP ( 'NONE', ( #20431, #5111, #22527, #13345 ) ) ;
#2662 = ORIENTED_EDGE ( 'NONE', *, *, #14826, .F. ) ;
#2663 = CARTESIAN_POINT ( 'NONE',  ( 43.31606138205700063, -21.31259689655800216, 45.10875082581016926 ) ) ;
#2664 = CARTESIAN_POINT ( 'NONE',  ( 38.26194895904383486, -1.013682088886101784, 69.64448340153879258 ) ) ;
#2665 = CARTESIAN_POINT ( 'NONE',  ( 37.80618814713138676, -27.70384086642190269, 69.62690120949091011 ) ) ;
#2666 = DIRECTION ( 'NONE',  ( 0.000000000000000000, -2.999999999999999839E-15, -1.000000000000000000 ) ) ;
#2667 = ADVANCED_FACE ( 'NONE', ( #7502 ), #7762, .F. ) ;
#2668 = CARTESIAN_POINT ( 'NONE',  ( 40.77203464402485622, -10.51368208888610312, 71.32335560751961623 ) ) ;
#2669 = DIRECTION ( 'NONE',  ( 0.000000000000000000, -6.938893903907222067E-15, 1.000000000000000000 ) ) ;
#2670 = DIRECTION ( 'NONE',  ( 1.000000000000000000, 3.021713267217945694E-15, 1.865775460081201246E-16 ) ) ;
#2671 = CARTESIAN_POINT ( 'NONE',  ( 32.81606138205700773, 36.92314894770293421, 79.37823623207323465 ) ) ;
#2672 = AXIS2_PLACEMENT_3D ( 'NONE', #13302, #25245, #25371 ) ;
#2673 = CARTESIAN_POINT ( 'NONE',  ( 39.65227363581001185, -29.06301577344905240, 69.84007905757066226 ) ) ;
#2674 = CARTESIAN_POINT ( 'NONE',  ( 40.64099152588522657, 1.392818861812999964, 83.30501292736997243 ) ) ;
#2675 = CARTESIAN_POINT ( 'NONE',  ( 38.31606138205700063, 42.51966564709218943, 72.30501292737018559 ) ) ;
#2676 = ORIENTED_EDGE ( 'NONE', *, *, #22313, .T. ) ;
#2677 = CYLINDRICAL_SURFACE ( 'NONE', #16859, 1.500000000000001332 ) ;
#2678 = CARTESIAN_POINT ( 'NONE',  ( 32.81606138205700773, 38.19123852234598360, 71.05501292736988717 ) ) ;
#2679 = ORIENTED_EDGE ( 'NONE', *, *, #22395, .T. ) ;
#2680 = ORIENTED_EDGE ( 'NONE', *, *, #4318, .F. ) ;
#2681 = CARTESIAN_POINT ( 'NONE',  ( 40.77203464402485622, -19.10384086642191193, 71.43714994484032843 ) ) ;
#2682 = CARTESIAN_POINT ( 'NONE',  ( 37.80618814713140097, -25.91368208888610880, 73.13360434286902034 ) ) ;
#2683 = PLANE ( 'NONE',  #14439 ) ;
#2684 = ADVANCED_FACE ( 'NONE', ( #3624 ), #23078, .T. ) ;
#2685 = EDGE_CURVE ( 'NONE', #21676, #24723, #1445, .T. ) ;
#2686 = CARTESIAN_POINT ( 'NONE',  ( 40.31606138205700063, 8.691238522346989015, 65.80501292736998664 ) ) ;
#2687 =( NAMED_UNIT ( * ) PLANE_ANGLE_UNIT ( ) SI_UNIT ( $, .RADIAN. ) );
#2688 = ORIENTED_EDGE ( 'NONE', *, *, #13968, .F. ) ;
#2689 = CARTESIAN_POINT ( 'NONE',  ( 33.56606138205700773, -34.55876147765400219, 74.30501292737011454 ) ) ;
#2690 = EDGE_CURVE ( 'NONE', #10464, #19274, #1940, .T. ) ;
#2691 = DIRECTION ( 'NONE',  ( 0.000000000000000000, 0.000000000000000000, -1.000000000000000000 ) ) ;
#2692 = CARTESIAN_POINT ( 'NONE',  ( 39.73277004305198545, -26.21368208888610951, 73.23812341099225875 ) ) ;
#2693 = DIRECTION ( 'NONE',  ( -1.000000000000000000, 0.000000000000000000, 0.000000000000000000 ) ) ;
#2694 = CARTESIAN_POINT ( 'NONE',  ( 42.68042513965293949, 15.19123852234701388, 73.80501292736995822 ) ) ;
#2695 = CARTESIAN_POINT ( 'NONE',  ( 37.69796330110504101, -7.113682088886100985, 69.66206559358663242 ) ) ;
#2696 = DIRECTION ( 'NONE',  ( 2.690219486203388234E-15, -0.8967398287344627850, -0.4425581086832399147 ) ) ;
#2697 = CARTESIAN_POINT ( 'NONE',  ( 38.37017380507020192, -22.01368208888611022, 73.11602215082116629 ) ) ;
#2698 = CARTESIAN_POINT ( 'NONE',  ( 44.71606138205697079, -3.195232061939673240, -6.457771442202879797 ) ) ;
#2699 = EDGE_CURVE ( 'NONE', #14226, #16502, #9576, .T. ) ;
#2700 = PLANE ( 'NONE',  #4278 ) ;
#2701 = CARTESIAN_POINT ( 'NONE',  ( 37.31647492878124694, -22.30384086642191122, 72.03616607671141026 ) ) ;
#2702 = CARTESIAN_POINT ( 'NONE',  ( 39.29254315202756231, -12.81368208888610383, 69.94417936956672577 ) ) ;
#2703 = CIRCLE ( 'NONE', #15053, 0.7500000000000008882 ) ;
#2704 = CARTESIAN_POINT ( 'NONE',  ( 43.31606138205695089, 3.741517323833267294, 2.753690589366190711 ) ) ;
#2705 = ORIENTED_EDGE ( 'NONE', *, *, #9826, .F. ) ;
#2706 = CARTESIAN_POINT ( 'NONE',  ( 37.80618814713138676, -13.70384086642190979, 69.62690120949091011 ) ) ;
#2707 = DIRECTION ( 'NONE',  ( 0.000000000000000000, 1.000000000000000000, 0.000000000000000000 ) ) ;
#2708 = CARTESIAN_POINT ( 'NONE',  ( 36.64852494920107517, -7.413682088886104360, 70.89533451361948835 ) ) ;
#2709 = ORIENTED_EDGE ( 'NONE', *, *, #24840, .F. ) ;
#2710 = CARTESIAN_POINT ( 'NONE',  ( 39.64521430340304420, -12.81368208888610383, 69.45876917294175712 ) ) ;
#2711 = ORIENTED_EDGE ( 'NONE', *, *, #14927, .F. ) ;
#2712 = LINE ( 'NONE', #23729, #19768 ) ;
#2713 = DIRECTION ( 'NONE',  ( 0.000000000000000000, 0.3299742535180963943, -0.9439899321577402969 ) ) ;
#2714 = CARTESIAN_POINT ( 'NONE',  ( 38.37017380507018771, -9.603840866421911926, 70.24448340153877268 ) ) ;
#2715 = CARTESIAN_POINT ( 'NONE',  ( 43.31606138205700063, -20.45664737071796324, 43.87694304485803798 ) ) ;
#2716 = EDGE_LOOP ( 'NONE', ( #23000, #13285, #5049, #13767 ) ) ;
#2717 = PLANE ( 'NONE',  #19942 ) ;
#2718 = DIRECTION ( 'NONE',  ( -1.000000000000000000, -1.734723475976804876E-16, 1.734723475976814737E-16 ) ) ;
#2719 = CARTESIAN_POINT ( 'NONE',  ( 39.12911128074872380, -25.50384086642191406, 69.06206559358663810 ) ) ;
#2720 = FACE_OUTER_BOUND ( 'NONE', #3411, .T. ) ;
#2721 = CARTESIAN_POINT ( 'NONE',  ( 36.64852494920107517, -27.41368208888610525, 70.89533451361945993 ) ) ;
#2722 = DIRECTION ( 'NONE',  ( -1.047880217021202589E-15, 0.4425581086832399147, -0.8967398287344627850 ) ) ;
#2723 = FACE_OUTER_BOUND ( 'NONE', #3679, .T. ) ;
#2724 = VERTEX_POINT ( 'NONE', #15354 ) ;
#2725 = DIRECTION ( 'NONE',  ( 0.000000000000000000, 1.000000000000000000, -3.469446951953613400E-15 ) ) ;
#2726 = DIRECTION ( 'NONE',  ( -1.734723475976804876E-16, 1.000000000000000000, 0.000000000000000000 ) ) ;
#2727 = EDGE_CURVE ( 'NONE', #2309, #19667, #11509, .T. ) ;
#2728 = CARTESIAN_POINT ( 'NONE',  ( 38.93415946300897446, -15.50384086642190695, 69.66206559358663242 ) ) ;
#2729 = AXIS2_PLACEMENT_3D ( 'NONE', #578, #14375, #12463 ) ;
#2730 = DIRECTION ( 'NONE',  ( 1.000000000000000000, 0.000000000000000000, 0.000000000000000000 ) ) ;
#2731 = CARTESIAN_POINT ( 'NONE',  ( 33.31606138205700773, 2.761903742731119049, 12.21527246050395377 ) ) ;
#2732 = VECTOR ( 'NONE', #21409, 1000.000000000000114 ) ;
#2733 = VECTOR ( 'NONE', #12443, 1000.000000000000000 ) ;
#2734 = CARTESIAN_POINT ( 'NONE',  ( 43.31606138205700773, -23.16691978223481385, 31.29201591705069063 ) ) ;
#2735 = DIRECTION ( 'NONE',  ( -0.000000000000000000, 1.000000000000000000, -3.225463739888140187E-15 ) ) ;
#2736 = CARTESIAN_POINT ( 'NONE',  ( 39.31564783533279694, 0.6961591335780878964, 70.72433947564853440 ) ) ;
#2737 = CARTESIAN_POINT ( 'NONE',  ( 37.42710149357921523, -5.397995270288631353, 82.79824951560235036 ) ) ;
#2738 = VERTEX_POINT ( 'NONE', #23593 ) ;
#2739 = CARTESIAN_POINT ( 'NONE',  ( 36.64852494920107517, -23.41368208888610525, 70.89533451361945993 ) ) ;
#2740 = ORIENTED_EDGE ( 'NONE', *, *, #17892, .F. ) ;
#2741 = ORIENTED_EDGE ( 'NONE', *, *, #9787, .F. ) ;
#2742 = CARTESIAN_POINT ( 'NONE',  ( 36.31606138205700063, 8.691238522346989015, 65.80501292736998664 ) ) ;
#2743 = CARTESIAN_POINT ( 'NONE',  ( 38.31606138205712853, 42.19123852234596939, 65.30501292736988717 ) ) ;
#2744 = CARTESIAN_POINT ( 'NONE',  ( 39.41296390513587511, -29.20384086642191335, 71.08074471024438878 ) ) ;
#2745 = CARTESIAN_POINT ( 'NONE',  ( 38.93987200065208754, -0.8136820888860993861, 70.42958956619168021 ) ) ;
#2746 = ORIENTED_EDGE ( 'NONE', *, *, #9299, .F. ) ;
#2747 = ORIENTED_EDGE ( 'NONE', *, *, #17523, .F. ) ;
#2748 = DIRECTION ( 'NONE',  ( 2.690219486203388234E-15, -0.8967398287344627850, -0.4425581086832399147 ) ) ;
#2749 = CARTESIAN_POINT ( 'NONE',  ( 43.06606138205700063, 41.44123852234599781, 74.30501292736987295 ) ) ;
#2750 = FACE_OUTER_BOUND ( 'NONE', #24828, .T. ) ;
#2751 = CARTESIAN_POINT ( 'NONE',  ( 39.98359781491296161, -11.20384086642191335, 70.89533451361947414 ) ) ;
#2752 = CLOSED_SHELL ( 'NONE', ( #8944, #6499, #5802, #8149, #15544, #6122, #16293, #22483, #5295, #15406, #19827, #21250, #19368, #23304, #25048, #16019, #16902, #9415, #15719, #5696, #23420, #5063, #20436, #5386, #1351, #506, #1901, #11860, #13780, #9037, #1032, #21074, #16026, #12568, #10832, #22777, #15249, #14248, #4837, #22034, #14011, #8171, #11324, #24115, #17290 ) ) ;
#2753 = VECTOR ( 'NONE', #14063, 1000.000000000000000 ) ;
#2754 = VECTOR ( 'NONE', #18406, 1000.000000000000114 ) ;
#2755 =( LENGTH_UNIT ( ) NAMED_UNIT ( * ) SI_UNIT ( .MILLI., .METRE. ) );
#2756 = CARTESIAN_POINT ( 'NONE',  ( 30.81606138205700418, 44.92314894770294131, 80.37823623207322044 ) ) ;
#2757 = VERTEX_POINT ( 'NONE', #15227 ) ;
#2758 = VERTEX_POINT ( 'NONE', #23205 ) ;
#2759 = VERTEX_POINT ( 'NONE', #19219 ) ;
#2760 = FACE_OUTER_BOUND ( 'NONE', #11147, .T. ) ;
#2761 = CARTESIAN_POINT ( 'NONE',  ( 36.49096545463212493, -5.513682088886105781, 71.43714994484035685 ) ) ;
#2762 = ADVANCED_FACE ( 'NONE', ( #15740 ), #5572, .T. ) ;
#2763 = ORIENTED_EDGE ( 'NONE', *, *, #11568, .F. ) ;
#2764 = DIRECTION ( 'NONE',  ( 0.000000000000000000, 2.999999999999999839E-15, 1.000000000000000000 ) ) ;
#2765 = DIRECTION ( 'NONE',  ( 1.734723475976804876E-16, 3.252606517456515274E-15, 1.000000000000000000 ) ) ;
#2766 = DIRECTION ( 'NONE',  ( 0.000000000000000000, 1.000000000000000000, -3.469446951953613400E-15 ) ) ;
#2767 = AXIS2_PLACEMENT_3D ( 'NONE', #14668, #24569, #10568 ) ;
#2768 = DIRECTION ( 'NONE',  ( 0.000000000000000000, 1.000000000000000000, -3.325260651745651169E-15 ) ) ;
#2769 = LINE ( 'NONE', #16829, #695 ) ;
#2770 = CIRCLE ( 'NONE', #8983, 1.499999999999994005 ) ;
#2771 = VECTOR ( 'NONE', #18659, 1000.000000000000000 ) ;
#2772 = DIRECTION ( 'NONE',  ( 1.958867181863079949E-15, -0.6529557272876933549, -0.7573960774932753104 ) ) ;
#2773 = ORIENTED_EDGE ( 'NONE', *, *, #21508, .T. ) ;
#2774 = ORIENTED_EDGE ( 'NONE', *, *, #25480, .F. ) ;
#2775 = CARTESIAN_POINT ( 'NONE',  ( 31.91606138205697363, -3.195232061939711432, -6.457771442202879797 ) ) ;
#2776 = CARTESIAN_POINT ( 'NONE',  ( 40.33642880535524000, -26.31368208888610383, 72.77780686321125359 ) ) ;
#2777 = EDGE_CURVE ( 'NONE', #24921, #120, #12252, .T. ) ;
#2778 = EDGE_CURVE ( 'NONE', #21084, #9967, #9825, .T. ) ;
#2779 = CARTESIAN_POINT ( 'NONE',  ( 38.93987200065208754, -26.81368208888610738, 70.42958956619166599 ) ) ;
#2780 = ORIENTED_EDGE ( 'NONE', *, *, #6442, .F. ) ;
#2781 = ORIENTED_EDGE ( 'NONE', *, *, #13984, .F. ) ;
#2782 = CARTESIAN_POINT ( 'NONE',  ( 36.31606138205700063, 5.691238522346988127, 65.30501292736998664 ) ) ;
#2783 = CARTESIAN_POINT ( 'NONE',  ( 36.49096545463212493, -1.513682088886105559, 71.43714994484035685 ) ) ;
#2784 = CARTESIAN_POINT ( 'NONE',  ( 38.82593461698265003, -28.70384086642190624, 73.13360434286902034 ) ) ;
#2785 = EDGE_CURVE ( 'NONE', #14994, #22403, #21662, .T. ) ;
#2786 = EDGE_CURVE ( 'NONE', #786, #13108, #25255, .T. ) ;
#2787 = EDGE_CURVE ( 'NONE', #11322, #11291, #11378, .T. ) ;
#2788 = CARTESIAN_POINT ( 'NONE',  ( 31.56606138205697576, -4.349482454670882348, -5.142398479549302515 ) ) ;
#2789 = CARTESIAN_POINT ( 'NONE',  ( 40.33642880535524000, -6.313682088886107380, 72.77780686321128201 ) ) ;
#2790 = VECTOR ( 'NONE', #13100, 1000.000000000000000 ) ;
#2791 = LINE ( 'NONE', #7191, #18097 ) ;
#2792 = AXIS2_PLACEMENT_3D ( 'NONE', #3118, #14843, #14713 ) ;
#2793 = VECTOR ( 'NONE', #4600, 1000.000000000000000 ) ;
#2794 = DIRECTION ( 'NONE',  ( 1.000000000000000000, 0.000000000000000000, 0.000000000000000000 ) ) ;
#2795 = EDGE_CURVE ( 'NONE', #14933, #23891, #24552, .T. ) ;
#2796 = CARTESIAN_POINT ( 'NONE',  ( 46.81606138205705037, -30.65246816789532502, 72.44500581826358143 ) ) ;
#2797 = EDGE_CURVE ( 'NONE', #24510, #23124, #12269, .T. ) ;
#2798 = DIRECTION ( 'NONE',  ( 1.000000000000000000, 1.000000000000000078E-15, 0.000000000000000000 ) ) ;
#2799 = LINE ( 'NONE', #2674, #18908 ) ;
#2800 = CARTESIAN_POINT ( 'NONE',  ( 44.71606138205697079, -3.854803714928911607, -5.706129749257958572 ) ) ;
#2801 = AXIS2_PLACEMENT_3D ( 'NONE', #4759, #500, #20478 ) ;
#2802 = CARTESIAN_POINT ( 'NONE',  ( 41.81606138205687273, 43.19123852234595518, 61.30501292736988006 ) ) ;
#2803 = ORIENTED_EDGE ( 'NONE', *, *, #5814, .F. ) ;
#2804 = CARTESIAN_POINT ( 'NONE',  ( 34.81606138205687273, 42.19123852234595518, 61.80501292736988006 ) ) ;
#2805 = CARTESIAN_POINT ( 'NONE',  ( 36.06606138205696510, -1.522470315718732037, 0.9921758631592225708 ) ) ;
#2806 = VERTEX_POINT ( 'NONE', #14442 ) ;
#2807 = EDGE_LOOP ( 'NONE', ( #24648, #21947 ) ) ;
#2808 = CARTESIAN_POINT ( 'NONE',  ( 35.86008812008917346, -16.10384086642191193, 71.32335560751961623 ) ) ;
#2809 = VECTOR ( 'NONE', #9333, 1000.000000000000000 ) ;
#2810 = CARTESIAN_POINT ( 'NONE',  ( 38.93415946300897446, -24.11368208888610454, 73.09843995877328382 ) ) ;
#2811 = DIRECTION ( 'NONE',  ( 0.000000000000000000, 0.000000000000000000, 1.000000000000000000 ) ) ;
#2812 = CARTESIAN_POINT ( 'NONE',  ( 32.81606138205700773, 22.19123852234699967, 69.30501292736994401 ) ) ;
#2813 = ORIENTED_EDGE ( 'NONE', *, *, #19782, .F. ) ;
#2814 = CARTESIAN_POINT ( 'NONE',  ( 41.14099152588522657, 1.392818861812999964, 83.30501292736997243 ) ) ;
#2815 = CARTESIAN_POINT ( 'NONE',  ( 36.31606138205700063, -29.30876147765401640, 69.30501292737010033 ) ) ;
#2816 = CARTESIAN_POINT ( 'NONE',  ( 38.26194895904383486, -27.01368208888609956, 69.04448340153878405 ) ) ;
#2817 = ORIENTED_EDGE ( 'NONE', *, *, #11715, .T. ) ;
#2818 = CARTESIAN_POINT ( 'NONE',  ( 43.81606138205700063, 6.355893005198818280, 6.643287643123708008 ) ) ;
#2819 = DIRECTION ( 'NONE',  ( 0.000000000000000000, 0.5706330172266919076, -0.8212051873014208914 ) ) ;
#2820 = CARTESIAN_POINT ( 'NONE',  ( 38.93415946300897446, -4.113682088886107202, 73.09843995877331224 ) ) ;
#2821 = DIRECTION ( 'NONE',  ( -2.727049986597864201E-15, 0.7516416929448760387, 0.6595716529892418079 ) ) ;
#2822 = CARTESIAN_POINT ( 'NONE',  ( 37.80618814713140097, -17.91368208888610525, 73.13360434286903455 ) ) ;
#2823 = CIRCLE ( 'NONE', #8627, 3.999999999999997335 ) ;
#2824 = FACE_OUTER_BOUND ( 'NONE', #2255, .T. ) ;
#2825 = LINE ( 'NONE', #18691, #10863 ) ;
#2826 = VECTOR ( 'NONE', #10298, 1000.000000000000000 ) ;
#2827 = CARTESIAN_POINT ( 'NONE',  ( 38.93987200065210175, -20.80384086642191122, 72.33091598616826445 ) ) ;
#2828 = CARTESIAN_POINT ( 'NONE',  ( 39.98359781491296161, -4.413682088886105248, 71.86517103874048473 ) ) ;
#2829 = DIRECTION ( 'NONE',  ( 7.071067811865460542E-16, -0.4341746501209495790, -0.9008287146801832179 ) ) ;
#2830 = PRODUCT_DEFINITION ( 'UNKNOWN', '', #24844, #11069 ) ;
#2831 = EDGE_LOOP ( 'NONE', ( #8003, #6092, #22375, #12048 ) ) ;
#2832 = AXIS2_PLACEMENT_3D ( 'NONE', #1094, #16828, #24412 ) ;
#2833 = CARTESIAN_POINT ( 'NONE',  ( 39.82603832034400426, -3.303840866421908995, 70.35351908239857721 ) ) ;
#2834 = DIRECTION ( 'NONE',  ( 0.000000000000000000, -0.7516416929448823669, -0.6595716529892345914 ) ) ;
#2835 = CARTESIAN_POINT ( 'NONE',  ( 36.64852494920107517, -5.413682088886106136, 70.89533451361948835 ) ) ;
#2836 = EDGE_LOOP ( 'NONE', ( #15757, #8570, #14018, #16670, #21693, #4211, #10031, #23447, #14005, #10769 ) ) ;
#2837 = CARTESIAN_POINT ( 'NONE',  ( 36.36258059203031934, -11.71368208888610951, 72.86986841596736042 ) ) ;
#2838 = ORIENTED_EDGE ( 'NONE', *, *, #6174, .T. ) ;
#2839 = DIRECTION ( 'NONE',  ( -1.000000000000000000, -1.734723475976814737E-16, 6.878321229954450795E-31 ) ) ;
#2840 = FACE_OUTER_BOUND ( 'NONE', #24503, .T. ) ;
#2841 = CARTESIAN_POINT ( 'NONE',  ( 38.00113996487112189, -13.70384086642191157, 70.22690120949090442 ) ) ;
#2842 = DIRECTION ( 'NONE',  ( 0.2503287245161955887, 0.9681609007195522976, -3.423740829372836395E-15 ) ) ;
#2843 = EDGE_LOOP ( 'NONE', ( #20394, #14541, #4813, #5088, #18954 ) ) ;
#2844 = DIRECTION ( 'NONE',  ( 2.758081859783345370E-15, -0.9193606199277819524, -0.3934158747763039088 ) ) ;
#2845 = CARTESIAN_POINT ( 'NONE',  ( 38.41621794735363693, -36.60729675983900222, 83.30501292737011454 ) ) ;
#2846 = CARTESIAN_POINT ( 'NONE',  ( 35.86008812008917346, -16.10384086642191193, 71.32335560751961623 ) ) ;
#2847 = VECTOR ( 'NONE', #13700, 1000.000000000000114 ) ;
#2848 = CARTESIAN_POINT ( 'NONE',  ( 37.31068429205632953, -21.96869763794396846, 75.81311457127152664 ) ) ;
#2849 = CYLINDRICAL_SURFACE ( 'NONE', #11187, 0.7500000000000006661 ) ;
#2850 = CARTESIAN_POINT ( 'NONE',  ( 37.25202387243752611, -21.21368208888610241, 70.00779233799262613 ) ) ;
#2851 = DIRECTION ( 'NONE',  ( 0.2672894156317878744, -0.9636162972320556630, 3.318080997173179155E-15 ) ) ;
#2852 = LINE ( 'NONE', #18974, #23354 ) ;
#2853 = AXIS2_PLACEMENT_3D ( 'NONE', #16665, #12814, #4810 ) ;
#2854 = ORIENTED_EDGE ( 'NONE', *, *, #24360, .T. ) ;
#2855 = DIRECTION ( 'NONE',  ( 1.000000000000000000, 1.734723475976804876E-16, -1.734723475976814737E-16 ) ) ;
#2856 = CARTESIAN_POINT ( 'NONE',  ( 38.31606138205700063, 38.69123852234599781, 71.30501292737000085 ) ) ;
#2857 = CARTESIAN_POINT ( 'NONE',  ( 36.80608444377002542, -12.30384086642191477, 72.40698646996133903 ) ) ;
#2858 = EDGE_CURVE ( 'NONE', #17088, #24765, #1120, .T. ) ;
#2859 = CARTESIAN_POINT ( 'NONE',  ( 39.31606138205700063, 43.19123852234599781, 75.30501292736987295 ) ) ;
#2860 = EDGE_CURVE ( 'NONE', #16500, #2274, #4004, .T. ) ;
#2861 = LINE ( 'NONE', #5074, #22572 ) ;
#2862 = CARTESIAN_POINT ( 'NONE',  ( 33.31606138205695089, 3.741517323833236208, 2.753690589366190711 ) ) ;
#2863 = CARTESIAN_POINT ( 'NONE',  ( 36.87297107704149823, -23.90384086642190198, 70.26145752964251301 ) ) ;
#2864 = CARTESIAN_POINT ( 'NONE',  ( 36.51585873400316018, -6.269293087353179139, 82.74377462301856667 ) ) ;
#2865 = EDGE_LOOP ( 'NONE', ( #9354, #11043, #24760, #8527 ) ) ;
#2866 = CIRCLE ( 'NONE', #6186, 1.000000000000000888 ) ;
#2867 = CARTESIAN_POINT ( 'NONE',  ( 40.14115730948191185, -24.51368208888609601, 71.32335560751958781 ) ) ;
#2868 = ORIENTED_EDGE ( 'NONE', *, *, #23949, .T. ) ;
#2869 = ORIENTED_EDGE ( 'NONE', *, *, #8023, .F. ) ;
#2870 = FACE_BOUND ( 'NONE', #22230, .T. ) ;
#2871 = CARTESIAN_POINT ( 'NONE',  ( 41.14099152588523367, -10.60718113818700026, 93.30501292736998664 ) ) ;
#2872 = VECTOR ( 'NONE', #15685, 1000.000000000000000 ) ;
#2873 = CARTESIAN_POINT ( 'NONE',  ( 39.31564783533280405, -2.313682088886100718, 72.03616607671141026 ) ) ;
#2874 = CARTESIAN_POINT ( 'NONE',  ( 37.31647492878122563, -1.313682088886099830, 70.72433947564853440 ) ) ;
#2875 = ORIENTED_EDGE ( 'NONE', *, *, #94, .T. ) ;
#2876 = VERTEX_POINT ( 'NONE', #13938 ) ;
#2877 = CARTESIAN_POINT ( 'NONE',  ( 33.56477571746443544, 3.418883076854447367, 6.349191931652266696 ) ) ;
#2878 = EDGE_CURVE ( 'NONE', #58, #2101, #22169, .T. ) ;
#2879 = CARTESIAN_POINT ( 'NONE',  ( 43.31606138205700063, -13.58280000135112964, 20.54174511886706256 ) ) ;
#2880 = VERTEX_POINT ( 'NONE', #16357 ) ;
#2881 = CARTESIAN_POINT ( 'NONE',  ( 47.84183937708599643, -34.55876147765400219, 70.30501292737000085 ) ) ;
#2882 = CARTESIAN_POINT ( 'NONE',  ( 38.37017380507018771, -7.603840866421906597, 69.64448340153879258 ) ) ;
#2883 = DIRECTION ( 'NONE',  ( 0.000000000000000000, 1.000000000000000000, 7.930164461608253340E-15 ) ) ;
#2884 = DIRECTION ( 'NONE',  ( 1.000000000000000000, 0.000000000000000000, 0.000000000000000000 ) ) ;
#2885 = ORIENTED_EDGE ( 'NONE', *, *, #2407, .F. ) ;
#2886 = EDGE_LOOP ( 'NONE', ( #15201, #16414, #12183, #5550, #21842, #864, #6325, #14118, #303 ) ) ;
#2887 = ORIENTED_EDGE ( 'NONE', *, *, #1881, .T. ) ;
#2888 = LINE ( 'NONE', #19379, #1350 ) ;
#2889 = VECTOR ( 'NONE', #10378, 1000.000000000000000 ) ;
#2890 = CARTESIAN_POINT ( 'NONE',  ( 39.38009889167650357, -2.213682088886108179, 72.75271321436733274 ) ) ;
#2891 = VERTEX_POINT ( 'NONE', #515 ) ;
#2892 = PLANE ( 'NONE',  #9807 ) ;
#2893 = PLANE ( 'NONE',  #19862 ) ;
#2894 = VECTOR ( 'NONE', #4752, 1000.000000000000114 ) ;
#2895 = ORIENTED_EDGE ( 'NONE', *, *, #22511, .F. ) ;
#2896 = DIRECTION ( 'NONE',  ( -1.000000000000000000, -2.168404344971010101E-16, 1.734723475976814737E-16 ) ) ;
#2897 = LINE ( 'NONE', #8596, #20978 ) ;
#2898 = DIRECTION ( 'NONE',  ( 1.000000000000000000, 1.115287202090205222E-30, -1.734723475976805122E-15 ) ) ;
#2899 = CARTESIAN_POINT ( 'NONE',  ( 34.81606138205696510, -1.316127829577488528, -4.808842309729777220 ) ) ;
#2900 = ORIENTED_EDGE ( 'NONE', *, *, #21220, .T. ) ;
#2901 = ORIENTED_EDGE ( 'NONE', *, *, #5341, .F. ) ;
#2902 = DIRECTION ( 'NONE',  ( 1.000000000000000000, 0.000000000000000000, 0.000000000000000000 ) ) ;
#2903 = DIRECTION ( 'NONE',  ( 1.000000000000000000, 0.000000000000000000, 0.000000000000000000 ) ) ;
#2905 = CIRCLE ( 'NONE', #4160, 1.750000000000001554 ) ;
#2904 = CARTESIAN_POINT ( 'NONE',  ( 39.37952058850012804, -18.61368208888609743, 70.97781676520601479 ) ) ;
#2906 = VERTEX_POINT ( 'NONE', #9952 ) ;
#2907 = ORIENTED_EDGE ( 'NONE', *, *, #20730, .T. ) ;
#2908 = EDGE_CURVE ( 'NONE', #9564, #7327, #10326, .T. ) ;
#2909 = CARTESIAN_POINT ( 'NONE',  ( 46.81606138205697221, -5.022037326221683529, -5.474317061061731771 ) ) ;
#2910 = ORIENTED_EDGE ( 'NONE', *, *, #12103, .T. ) ;
#2911 = CARTESIAN_POINT ( 'NONE',  ( 38.37017380507020192, -2.013682088886109334, 73.11602215082118050 ) ) ;
#2912 = CARTESIAN_POINT ( 'NONE',  ( 38.82593461698265003, -26.70384086642190624, 73.13360434286902034 ) ) ;
#2913 = VECTOR ( 'NONE', #10280, 1000.000000000000000 ) ;
#2914 = DIRECTION ( 'NONE',  ( 1.000000000000000000, 0.000000000000000000, 0.000000000000000000 ) ) ;
#2915 = CARTESIAN_POINT ( 'NONE',  ( 39.12911128074873801, -10.11368208888610987, 73.69843995877330656 ) ) ;
#2916 = CARTESIAN_POINT ( 'NONE',  ( 40.31606138205700773, -1.357181138186128067, 82.80501292736991559 ) ) ;
#2917 = CARTESIAN_POINT ( 'NONE',  ( 40.30346352106939634, -6.945422957003676956, 83.16042775478545934 ) ) ;
#2918 = DIRECTION ( 'NONE',  ( 2.690219486203388234E-15, -0.8967398287344627850, -0.4425581086832399147 ) ) ;
#2919 = CARTESIAN_POINT ( 'NONE',  ( 29.81606138205706458, -34.13844651005150155, 70.48338531520533934 ) ) ;
#2920 = EDGE_CURVE ( 'NONE', #9149, #30, #21694, .T. ) ;
#2921 = EDGE_CURVE ( 'NONE', #16440, #13002, #12398, .T. ) ;
#2922 = CARTESIAN_POINT ( 'NONE',  ( 38.96303889229209716, -5.302259509207527088, 82.79964613853329070 ) ) ;
#2923 = CARTESIAN_POINT ( 'NONE',  ( 34.81606138205696510, -0.8482369431493941292, -3.067843137301039302 ) ) ;
#2924 = EDGE_CURVE ( 'NONE', #12220, #11300, #22115, .T. ) ;
#2925 = EDGE_CURVE ( 'NONE', #19241, #4343, #13082, .T. ) ;
#2926 = LINE ( 'NONE', #18534, #16420 ) ;
#2927 = EDGE_CURVE ( 'NONE', #12825, #17958, #1945, .T. ) ;
#2928 = VERTEX_POINT ( 'NONE', #2323 ) ;
#2929 = CARTESIAN_POINT ( 'NONE',  ( 39.53940869104339839, -21.80867927670156803, 75.30820817392812216 ) ) ;
#2930 = PRESENTATION_LAYER_ASSIGNMENT (  '', '', ( #16512 ) ) ;
#2931 = DIRECTION ( 'NONE',  ( 1.000000000000000000, 0.000000000000000000, 0.000000000000000000 ) ) ;
#2932 = ORIENTED_EDGE ( 'NONE', *, *, #16638, .T. ) ;
#2933 = ORIENTED_EDGE ( 'NONE', *, *, #22167, .F. ) ;
#2934 = CARTESIAN_POINT ( 'NONE',  ( 40.33642880535521869, -19.30384086642191477, 69.98269868914866265 ) ) ;
#2935 = ADVANCED_FACE ( 'NONE', ( #10199 ), #14315, .T. ) ;
#2936 = CARTESIAN_POINT ( 'NONE',  ( 36.49096545463212493, -23.51368208888609601, 71.43714994484030001 ) ) ;
#2937 = DIRECTION ( 'NONE',  ( 0.000000000000000000, 0.7540134720837717852, 0.6568589528324745297 ) ) ;
#2938 = EDGE_CURVE ( 'NONE', #14856, #17225, #638, .T. ) ;
#2939 = CARTESIAN_POINT ( 'NONE',  ( 31.81606138205700418, -38.55876147765410167, 72.21586839016146087 ) ) ;
#2940 = PRESENTATION_STYLE_ASSIGNMENT (( #20609 ) ) ;
#2941 = ORIENTED_EDGE ( 'NONE', *, *, #898, .T. ) ;
#2942 = CARTESIAN_POINT ( 'NONE',  ( 40.81606138205700773, -29.78523130861184143, 52.92072663988442116 ) ) ;
#2943 = CARTESIAN_POINT ( 'NONE',  ( 47.81606138205695089, -23.19619402982945644, 47.16846523730003327 ) ) ;
#2944 = CARTESIAN_POINT ( 'NONE',  ( 36.07789103942398867, -27.41368208888610525, 70.70992431699450265 ) ) ;
#2945 = VECTOR ( 'NONE', #9886, 1000.000000000000227 ) ;
#2946 = VERTEX_POINT ( 'NONE', #6582 ) ;
#2947 = AXIS2_PLACEMENT_3D ( 'NONE', #6664, #18149, #4614 ) ;
#2948 = CARTESIAN_POINT ( 'NONE',  ( 45.81606138205700063, -34.55876147765410167, 66.30501292737000085 ) ) ;
#2949 = CARTESIAN_POINT ( 'NONE',  ( 36.68196826583682935, -3.613682088886103205, 71.96809898377890136 ) ) ;
#2950 = LINE ( 'NONE', #24581, #21507 ) ;
#2951 = VECTOR ( 'NONE', #10283, 1000.000000000000000 ) ;
#2952 = CARTESIAN_POINT ( 'NONE',  ( 36.80608444377001121, -17.31368208888610027, 70.35351908239860563 ) ) ;
#2953 = CARTESIAN_POINT ( 'NONE',  ( 38.31606138205700063, -22.22127907754186893, 75.80501292736997243 ) ) ;
#2954 = DIRECTION ( 'NONE',  ( 0.000000000000000000, 1.000000000000000000, -2.999999999999998655E-15 ) ) ;
#2955 = EDGE_CURVE ( 'NONE', #8986, #12061, #11890, .T. ) ;
#2956 = CARTESIAN_POINT ( 'NONE',  ( 37.38336156205273397, -19.90384086642191264, 70.63227792289247020 ) ) ;
#2957 = CARTESIAN_POINT ( 'NONE',  ( 39.82603832034400426, -4.313682088886107380, 72.40698646996135324 ) ) ;
#2958 = EDGE_CURVE ( 'NONE', #3261, #24591, #144, .T. ) ;
#2959 = ORIENTED_EDGE ( 'NONE', *, *, #22645, .T. ) ;
#2960 = CARTESIAN_POINT ( 'NONE',  ( 35.64099152588522657, -1.357181138186998925, 80.05501292737000085 ) ) ;
#2961 = ORIENTED_EDGE ( 'NONE', *, *, #21508, .F. ) ;
#2962 = CARTESIAN_POINT ( 'NONE',  ( 37.33957961208645315, -7.803840866421909439, 69.94417936956673998 ) ) ;
#2963 = CARTESIAN_POINT ( 'NONE',  ( 40.31606138205700773, -20.32127907754186680, 75.99695190479390305 ) ) ;
#2964 = CIRCLE ( 'NONE', #1737, 10.00000000000000178 ) ;
#2965 = ADVANCED_FACE ( 'NONE', ( #6079 ), #23962, .T. ) ;
#2966 = CARTESIAN_POINT ( 'NONE',  ( 39.95015449827720744, -6.613682088886106314, 70.79240656858107172 ) ) ;
#2967 = ORIENTED_EDGE ( 'NONE', *, *, #1092, .T. ) ;
#2968 = CARTESIAN_POINT ( 'NONE',  ( 39.12911128074873801, -8.113682088886108090, 73.69843995877330656 ) ) ;
#2969 = VERTEX_POINT ( 'NONE', #12020 ) ;
#2970 = DIRECTION ( 'NONE',  ( 4.341746501209495972E-16, -0.4341746501209495790, -0.9008287146801833289 ) ) ;
#2971 = CARTESIAN_POINT ( 'NONE',  ( 37.89291511884479036, -10.50384086642191050, 72.49843995877331793 ) ) ;
#2972 = CARTESIAN_POINT ( 'NONE',  ( 45.81606138205697221, -4.589472609077215104, -6.350807634294793225 ) ) ;
#2973 = EDGE_LOOP ( 'NONE', ( #14866, #6361, #19579, #5404 ) ) ;
#2974 = CIRCLE ( 'NONE', #15738, 0.7499999999999996669 ) ;
#2975 = DIRECTION ( 'NONE',  ( -1.000000000000000000, -1.734723475976804876E-16, 1.734723475976814737E-16 ) ) ;
#2976 = CARTESIAN_POINT ( 'NONE',  ( 43.31606138205700063, -14.32738121993773994, 11.12118157620986558 ) ) ;
#2977 = CARTESIAN_POINT ( 'NONE',  ( 36.98690846071097127, -15.80384086642191299, 69.45876917294175712 ) ) ;
#2978 = VECTOR ( 'NONE', #19951, 1000.000000000000000 ) ;
#2979 = CARTESIAN_POINT ( 'NONE',  ( 40.31606138205700773, 38.69123852234599781, 75.30501292737004349 ) ) ;
#2980 = CARTESIAN_POINT ( 'NONE',  ( 37.69796330110504101, -21.11368208888610454, 69.66206559358661821 ) ) ;
#2981 = CARTESIAN_POINT ( 'NONE',  ( 44.06606138205700063, 43.35512946304240245, 83.12823623207320622 ) ) ;
#2982 = EDGE_CURVE ( 'NONE', #7462, #1147, #19860, .T. ) ;
#2983 = AXIS2_PLACEMENT_3D ( 'NONE', #20163, #8189, #565 ) ;
#2984 = DIRECTION ( 'NONE',  ( 1.327674326049719602E-15, -0.4425581086832399147, 0.8967398287344627850 ) ) ;
#2985 = VECTOR ( 'NONE', #17332, 1000.000000000000000 ) ;
#2986 = VERTEX_POINT ( 'NONE', #10083 ) ;
#2987 = PLANE ( 'NONE',  #16591 ) ;
#2988 = FACE_OUTER_BOUND ( 'NONE', #3836, .T. ) ;
#2989 = AXIS2_PLACEMENT_3D ( 'NONE', #7407, #3271, #22854 ) ;
#2990 = CARTESIAN_POINT ( 'NONE',  ( 39.29254315202757653, -12.80384086642191299, 72.81632618279321889 ) ) ;
#2991 = DIRECTION ( 'NONE',  ( 1.000000000000000000, 0.000000000000000000, 0.000000000000000000 ) ) ;
#2992 = CYLINDRICAL_SURFACE ( 'NONE', #14533, 1.000000000000000888 ) ;
#2993 = CARTESIAN_POINT ( 'NONE',  ( 39.98359781491296161, -24.41368208888610525, 71.86517103874045631 ) ) ;
#2994 = CARTESIAN_POINT ( 'NONE',  ( 33.31606138205700773, -21.50052602411404834, 44.06487217241408416 ) ) ;
#2995 = VECTOR ( 'NONE', #19543, 1000.000000000000227 ) ;
#2996 = CARTESIAN_POINT ( 'NONE',  ( 39.98359781491296161, -23.20384086642191335, 70.89533451361945993 ) ) ;
#2997 = CARTESIAN_POINT ( 'NONE',  ( 36.31606138205700063, -7.108002773205779334, 82.61702262452435264 ) ) ;
#2998 = CARTESIAN_POINT ( 'NONE',  ( 36.49096545463212493, -25.51368208888609956, 71.43714994484030001 ) ) ;
#2999 = ORIENTED_EDGE ( 'NONE', *, *, #1378, .T. ) ;
#3000 = EDGE_LOOP ( 'NONE', ( #2526, #7354, #10115, #4750 ) ) ;
#3001 = DIRECTION ( 'NONE',  ( 1.156482317317872711E-16, 0.4425581086832400257, -0.8967398287344628960 ) ) ;
#3002 = VECTOR ( 'NONE', #12937, 1000.000000000000227 ) ;
#3003 = DIRECTION ( 'NONE',  ( 0.000000000000000000, -6.938893903907222067E-15, 1.000000000000000000 ) ) ;
#3004 = CARTESIAN_POINT ( 'NONE',  ( 39.02742774030102879, 1.786317911113898704, 72.26730301774236409 ) ) ;
#3005 = CARTESIAN_POINT ( 'NONE',  ( 39.37952058850012804, -29.00384086642191406, 71.78268878715390144 ) ) ;
#3006 = EDGE_LOOP ( 'NONE', ( #703, #13380, #8247, #6877 ) ) ;
#3007 = ORIENTED_EDGE ( 'NONE', *, *, #25106, .F. ) ;
#3008 = DIRECTION ( 'NONE',  ( 0.000000000000000000, 0.000000000000000000, 1.000000000000000000 ) ) ;
#3009 = VECTOR ( 'NONE', #8392, 1000.000000000000000 ) ;
#3010 = FACE_OUTER_BOUND ( 'NONE', #13087, .T. ) ;
#3011 = ORIENTED_EDGE ( 'NONE', *, *, #12594, .T. ) ;
#3012 =( NAMED_UNIT ( * ) SI_UNIT ( $, .STERADIAN. ) SOLID_ANGLE_UNIT ( ) );
#3013 = CARTESIAN_POINT ( 'NONE',  ( 38.82593461698265003, -4.703840866421914235, 73.13360434286904876 ) ) ;
#3014 = EDGE_CURVE ( 'NONE', #4268, #13492, #16450, .T. ) ;
#3015 = EDGE_CURVE ( 'NONE', #3872, #13887, #6580, .T. ) ;
#3016 = CARTESIAN_POINT ( 'NONE',  ( 32.81606138205700773, -2.373793412309109563, 19.60611914621674146 ) ) ;
#3017 = VECTOR ( 'NONE', #11670, 1000.000000000000114 ) ;
#3018 = EDGE_CURVE ( 'NONE', #25424, #11314, #24461, .T. ) ;
#3019 = CARTESIAN_POINT ( 'NONE',  ( 43.31606138205700063, -5.204193249396356968, 72.80501292736992980 ) ) ;
#3020 = ORIENTED_EDGE ( 'NONE', *, *, #3910, .T. ) ;
#3021 = ORIENTED_EDGE ( 'NONE', *, *, #1196, .F. ) ;
#3022 = ORIENTED_EDGE ( 'NONE', *, *, #8029, .F. ) ;
#3023 = DIRECTION ( 'NONE',  ( 1.000000000000000000, 4.336808689942014655E-17, -1.734723475976809806E-16 ) ) ;
#3024 = CARTESIAN_POINT ( 'NONE',  ( 36.80608444377001121, -3.313682088886101162, 70.35351908239861984 ) ) ;
#3025 = ORIENTED_EDGE ( 'NONE', *, *, #3131, .T. ) ;
#3026 = CARTESIAN_POINT ( 'NONE',  ( 33.31606138205700773, -29.06829118875199924, 75.80501292737000085 ) ) ;
#3027 = CIRCLE ( 'NONE', #19491, 1.000000000000000888 ) ;
#3028 = CARTESIAN_POINT ( 'NONE',  ( 36.31606138205700063, 37.94123852234599781, 74.30501292736988717 ) ) ;
#3029 = DIRECTION ( 'NONE',  ( 0.000000000000000000, -3.469446951953613400E-15, -1.000000000000000000 ) ) ;
#3030 = EDGE_CURVE ( 'NONE', #7575, #19237, #18812, .T. ) ;
#3031 = CIRCLE ( 'NONE', #18669, 3.999999999999997335 ) ;
#3032 = LINE ( 'NONE', #16384, #19445 ) ;
#3033 = CARTESIAN_POINT ( 'NONE',  ( 33.81606138205700063, 22.19123852234699967, 69.30501292736994401 ) ) ;
#3034 = CARTESIAN_POINT ( 'NONE',  ( 37.01167919801150674, -5.663575426409370728, 82.79453121852071718 ) ) ;
#3035 = FACE_OUTER_BOUND ( 'NONE', #20986, .T. ) ;
#3036 = ORIENTED_EDGE ( 'NONE', *, *, #5474, .F. ) ;
#3037 = ORIENTED_EDGE ( 'NONE', *, *, #7448, .F. ) ;
#3038 = LINE ( 'NONE', #16962, #4625 ) ;
#3039 = DIRECTION ( 'NONE',  ( -1.327674326049719602E-15, 0.4425581086832399147, -0.8967398287344627850 ) ) ;
#3040 =( REPRESENTATION_RELATIONSHIP ('NONE','NONE', #17377, #14587 ) REPRESENTATION_RELATIONSHIP_WITH_TRANSFORMATION ( #15982 )SHAPE_REPRESENTATION_RELATIONSHIP( ) );
#3041 =( GEOMETRIC_REPRESENTATION_CONTEXT ( 3 ) GLOBAL_UNCERTAINTY_ASSIGNED_CONTEXT ( ( #24699 ) ) GLOBAL_UNIT_ASSIGNED_CONTEXT ( ( #5109, #483, #22135 ) ) REPRESENTATION_CONTEXT ( 'NONE', 'WORKASPACE' ) );
#3042 = CARTESIAN_POINT ( 'NONE',  ( 39.51027997493896748, -18.51368208888610312, 71.32335560751960202 ) ) ;
#3043 = VERTEX_POINT ( 'NONE', #14563 ) ;
#3044 = ORIENTED_EDGE ( 'NONE', *, *, #18005, .T. ) ;
#3045 = FACE_OUTER_BOUND ( 'NONE', #25037, .T. ) ;
#3046 = CARTESIAN_POINT ( 'NONE',  ( 36.64852494920107517, -3.413682088886104360, 70.89533451361948835 ) ) ;
#3047 = CARTESIAN_POINT ( 'NONE',  ( 37.69796330110505522, -22.50384086642191050, 73.09843995877329803 ) ) ;
#3048 = CIRCLE ( 'NONE', #6776, 1.000000000000000888 ) ;
#3049 = AXIS2_PLACEMENT_3D ( 'NONE', #8952, #9089, #8704 ) ;
#3050 = DIRECTION ( 'NONE',  ( 0.000000000000000000, 1.000000000000000000, -2.999999999999999839E-15 ) ) ;
#3051 = PRESENTATION_LAYER_ASSIGNMENT (  '', '', ( #8422 ) ) ;
#3052 = CARTESIAN_POINT ( 'NONE',  ( 40.55423172469004811, -8.413682088886105248, 72.05058123536544201 ) ) ;
#3053 = FACE_OUTER_BOUND ( 'NONE', #17960, .T. ) ;
#3054 = ORIENTED_EDGE ( 'NONE', *, *, #14434, .T. ) ;
#3055 = CARTESIAN_POINT ( 'NONE',  ( 39.54057891361352972, -5.617364314676576598, 83.29713963190137349 ) ) ;
#3056 = CARTESIAN_POINT ( 'NONE',  ( 36.31606138205700063, -20.32127907754186680, 75.99695190479390305 ) ) ;
#3057 = CARTESIAN_POINT ( 'NONE',  ( 32.81606138205700773, -35.70002751211045933, 71.94742330197156832 ) ) ;
#3058 = VERTEX_POINT ( 'NONE', #8642 ) ;
#3059 = CARTESIAN_POINT ( 'NONE',  ( 40.21566563214662438, -6.500168537627977194, 82.72135851617947822 ) ) ;
#3060 = LINE ( 'NONE', #10936, #6085 ) ;
#3061 = ADVANCED_FACE ( 'NONE', ( #3088 ), #14685, .T. ) ;
#3062 = DIRECTION ( 'NONE',  ( -1.734723475976804876E-16, -3.269436733918100469E-15, -1.000000000000000000 ) ) ;
#3063 = ORIENTED_EDGE ( 'NONE', *, *, #3083, .T. ) ;
#3064 = CARTESIAN_POINT ( 'NONE',  ( 41.31606138205700063, 7.187001342539796944, 66.09667597968754649 ) ) ;
#3065 = DIRECTION ( 'NONE',  ( 1.000000000000000000, 0.000000000000000000, 0.000000000000000000 ) ) ;
#3066 = VERTEX_POINT ( 'NONE', #16490 ) ;
#3067 = AXIS2_PLACEMENT_3D ( 'NONE', #2981, #12801, #8814 ) ;
#3068 = ORIENTED_EDGE ( 'NONE', *, *, #18672, .T. ) ;
#3069 = UNCERTAINTY_MEASURE_WITH_UNIT (LENGTH_MEASURE( 1.000000000000000082E-05 ), #19515, 'distance_accuracy_value', 'NONE');
#3070 = CARTESIAN_POINT ( 'NONE',  ( 36.29569395875881099, -20.30384086642191122, 72.77780686321128201 ) ) ;
#3071 = CARTESIAN_POINT ( 'NONE',  ( 38.37017380507020192, -24.01368208888610667, 73.11602215082115208 ) ) ;
#3072 = LINE ( 'NONE', #5016, #12394 ) ;
#3073 = EDGE_CURVE ( 'NONE', #6274, #19237, #5359, .T. ) ;
#3074 = DIRECTION ( 'NONE',  ( 1.000000000000000000, 2.602085213965208275E-15, 0.000000000000000000 ) ) ;
#3075 = EDGE_CURVE ( 'NONE', #3766, #18371, #14947, .T. ) ;
#3076 = EDGE_LOOP ( 'NONE', ( #12755, #11807, #21212, #5375 ) ) ;
#3077 = DIRECTION ( 'NONE',  ( -1.000000000000000000, -6.938893903907222067E-15, 0.000000000000000000 ) ) ;
#3078 = CARTESIAN_POINT ( 'NONE',  ( 36.31606138205700063, -12.76023008545320714, 21.53290024082827969 ) ) ;
#3079 = CARTESIAN_POINT ( 'NONE',  ( 39.02088643472237095, -28.91368208888610170, 69.02690120949091579 ) ) ;
#3080 = VECTOR ( 'NONE', #19562, 1000.000000000000000 ) ;
#3081 = EDGE_LOOP ( 'NONE', ( #23010, #5207, #12290, #19264, #406, #13889, #20963, #24163, #19020, #5502, #9015, #15641, #6393, #18770, #23900, #13377, #22253, #814, #10760 ) ) ;
#3082 = VECTOR ( 'NONE', #636, 1000.000000000000000 ) ;
#3083 = EDGE_CURVE ( 'NONE', #4595, #4703, #12650, .T. ) ;
#3084 = DIRECTION ( 'NONE',  ( 0.000000000000000000, -1.000000000000000000, 4.625929269271485322E-15 ) ) ;
#3085 = CARTESIAN_POINT ( 'NONE',  ( 38.26194895904383486, 0.9863179111138999922, 69.64448340153880679 ) ) ;
#3086 = CARTESIAN_POINT ( 'NONE',  ( 35.64099152588522657, 1.142818861812999742, 82.55501292736997243 ) ) ;
#3087 = CARTESIAN_POINT ( 'NONE',  ( 36.87297107704153376, -19.71368208888610951, 72.49904802271740323 ) ) ;
#3088 = FACE_OUTER_BOUND ( 'NONE', #13458, .T. ) ;
#3089 = EDGE_CURVE ( 'NONE', #2986, #5253, #14766, .T. ) ;
#3090 = FACE_BOUND ( 'NONE', #6509, .T. ) ;
#3091 = CARTESIAN_POINT ( 'NONE',  ( 38.93987200065210175, -16.80384086642191477, 72.33091598616826445 ) ) ;
#3092 = CARTESIAN_POINT ( 'NONE',  ( 39.95015449827720744, -4.613682088886104538, 70.79240656858107172 ) ) ;
#3093 = CARTESIAN_POINT ( 'NONE',  ( 39.92124728212843365, -21.44350662387563489, 75.33352358636996371 ) ) ;
#3094 = ORIENTED_EDGE ( 'NONE', *, *, #9813, .F. ) ;
#3095 = CARTESIAN_POINT ( 'NONE',  ( 38.26194895904384907, -2.603840866421916367, 73.11602215082118050 ) ) ;
#3096 = LINE ( 'NONE', #16249, #7363 ) ;
#3097 = CARTESIAN_POINT ( 'NONE',  ( 38.93415946300897446, -6.113682088886107202, 73.09843995877331224 ) ) ;
#3098 = EDGE_LOOP ( 'NONE', ( #5356, #25164, #8587, #6818 ) ) ;
#3099 = PRODUCT_DEFINITION_SHAPE ( 'NONE', 'NONE',  #25497 ) ;
#3100 = CARTESIAN_POINT ( 'NONE',  ( 36.11133435605973574, -9.613682088886104538, 72.15350918040385864 ) ) ;
#3101 = ORIENTED_EDGE ( 'NONE', *, *, #20873, .F. ) ;
#3102 = PLANE ( 'NONE',  #1249 ) ;
#3103 = CARTESIAN_POINT ( 'NONE',  ( 37.12184278917507640, -14.10384086642191370, 71.32335560751961623 ) ) ;
#3104 = EDGE_CURVE ( 'NONE', #14953, #4563, #18947, .T. ) ;
#3105 = CARTESIAN_POINT ( 'NONE',  ( 32.56606138205700773, 41.63025572888945192, 83.79244979444629848 ) ) ;
#3106 = EDGE_CURVE ( 'NONE', #15655, #12192, #22421, .T. ) ;
#3107 = ORIENTED_EDGE ( 'NONE', *, *, #18870, .T. ) ;
#3108 = DIRECTION ( 'NONE',  ( 1.849283715844614949E-16, -0.8212051873014210024, -0.5706330172266920187 ) ) ;
#3109 = CARTESIAN_POINT ( 'NONE',  ( 33.31606138205700773, -20.88462213363798270, 44.49284693533410717 ) ) ;
#3110 = CARTESIAN_POINT ( 'NONE',  ( 36.07789103942399578, -18.20384086642191690, 72.05058123536544201 ) ) ;
#3111 = ADVANCED_FACE ( 'NONE', ( #2824 ), #6704, .T. ) ;
#3112 = EDGE_CURVE ( 'NONE', #17565, #20324, #12778, .T. ) ;
#3113 = EDGE_CURVE ( 'NONE', #3872, #15753, #9022, .T. ) ;
#3114 = CARTESIAN_POINT ( 'NONE',  ( 36.99021717747880444, -21.72436795495472950, 75.31693369342355027 ) ) ;
#3115 = CARTESIAN_POINT ( 'NONE',  ( 43.31606138205700773, -19.34822312381089660, 24.15308711316412627 ) ) ;
#3116 = CARTESIAN_POINT ( 'NONE',  ( 39.82603832034400426, -22.31368208888610738, 72.40698646996133903 ) ) ;
#3117 = DIRECTION ( 'NONE',  ( -1.734723475976804876E-16, 1.000000000000000000, 0.000000000000000000 ) ) ;
#3118 = CARTESIAN_POINT ( 'NONE',  ( 36.31606138205700063, 37.94123852234599070, 73.55501292736988717 ) ) ;
#3119 = VERTEX_POINT ( 'NONE', #7223 ) ;
#3120 = ORIENTED_EDGE ( 'NONE', *, *, #12244, .F. ) ;
#3121 = DIRECTION ( 'NONE',  ( -1.734723475976804876E-16, 1.000000000000000000, 0.000000000000000000 ) ) ;
#3122 = CARTESIAN_POINT ( 'NONE',  ( 35.91606138205695942, 0.5799492015812600654, -3.145019409304214530 ) ) ;
#3123 = CARTESIAN_POINT ( 'NONE',  ( 36.80608444377002542, -10.30384086642191299, 72.40698646996135324 ) ) ;
#3125 = EDGE_CURVE ( 'NONE', #24795, #21810, #17458, .T. ) ;
#3124 = DIRECTION ( 'NONE',  ( 1.000000000000000000, 0.000000000000000000, 0.000000000000000000 ) ) ;
#3126 = CARTESIAN_POINT ( 'NONE',  ( 30.81606138205700418, -8.607181138186998481, 79.30501292737000085 ) ) ;
#3127 = CARTESIAN_POINT ( 'NONE',  ( 39.95015449827720744, -22.61368208888610809, 70.79240656858105751 ) ) ;
#3128 = CARTESIAN_POINT ( 'NONE',  ( 31.81606138205700418, 41.44123852234595518, 61.30501292736988006 ) ) ;
#3129 = CARTESIAN_POINT ( 'NONE',  ( 38.82593461698265003, -22.70384086642191690, 73.13360434286903455 ) ) ;
#3130 = LINE ( 'NONE', #4575, #2733 ) ;
#3131 = EDGE_CURVE ( 'NONE', #15899, #16389, #25430, .T. ) ;
#3132 = CARTESIAN_POINT ( 'NONE',  ( 39.75915168707250302, -26.71368208888609530, 70.26145752964249880 ) ) ;
#3133 = ORIENTED_EDGE ( 'NONE', *, *, #21482, .T. ) ;
#3134 = ORIENTED_EDGE ( 'NONE', *, *, #5824, .F. ) ;
#3135 = CARTESIAN_POINT ( 'NONE',  ( 33.23698182036294924, 3.107175835156888333, 6.136003935501333828 ) ) ;
#3136 = CARTESIAN_POINT ( 'NONE',  ( 32.81606138205700773, -20.88462213363798270, 44.49284693533410717 ) ) ;
#3137 = CARTESIAN_POINT ( 'NONE',  ( 39.51027997493896748, -29.10384086642191193, 71.43714994484031422 ) ) ;
#3138 = CARTESIAN_POINT ( 'NONE',  ( 39.41296390513587511, -0.4136820888861019174, 71.67976084211552745 ) ) ;
#3139 = ORIENTED_EDGE ( 'NONE', *, *, #5484, .T. ) ;
#3140 = VERTEX_POINT ( 'NONE', #24965 ) ;
#3141 = CARTESIAN_POINT ( 'NONE',  ( 46.81606138205696510, -2.286980848581572356, -4.124514829577853980 ) ) ;
#3142 = DIRECTION ( 'NONE',  ( 1.000000000000000000, 2.999999999999999839E-15, 0.000000000000000000 ) ) ;
#3143 = ORIENTED_EDGE ( 'NONE', *, *, #18547, .T. ) ;
#3144 = CARTESIAN_POINT ( 'NONE',  ( 45.81606138205705037, -30.65246816789533213, 72.44500581826358143 ) ) ;
#3145 = CARTESIAN_POINT ( 'NONE',  ( 38.37017380507018771, -3.603840866421907041, 69.64448340153879258 ) ) ;
#3146 = CARTESIAN_POINT ( 'NONE',  ( 40.31606138205700773, 8.691238522346985462, 65.51211970855652567 ) ) ;
#3147 = FACE_OUTER_BOUND ( 'NONE', #2379, .T. ) ;
#3148 = ORIENTED_EDGE ( 'NONE', *, *, #12027, .F. ) ;
#3149 = ORIENTED_EDGE ( 'NONE', *, *, #8029, .T. ) ;
#3150 = CARTESIAN_POINT ( 'NONE',  ( 35.31606138205700773, 9.119667998728431257, 66.98393923633439329 ) ) ;
#3151 = CARTESIAN_POINT ( 'NONE',  ( 39.75915168707250302, -2.713682088886101962, 70.26145752964255564 ) ) ;
#3152 = EDGE_LOOP ( 'NONE', ( #22051, #19916, #9029, #12464 ) ) ;
#3153 = CARTESIAN_POINT ( 'NONE',  ( 39.82603832034401137, -25.30384086642190766, 70.35351908239857721 ) ) ;
#3154 = DIRECTION ( 'NONE',  ( 0.000000000000000000, -1.000000000000000000, 0.000000000000000000 ) ) ;
#3155 = VERTEX_POINT ( 'NONE', #19437 ) ;
#3156 = DIRECTION ( 'NONE',  ( -2.048868001712898319E-15, 0.6595716529892350355, -0.7516416929448821449 ) ) ;
#3157 = DIRECTION ( 'NONE',  ( -1.734723475976814737E-16, 1.000000000000000000, -3.491481338843135327E-15 ) ) ;
#3158 = EDGE_CURVE ( 'NONE', #25244, #17225, #11738, .T. ) ;
#3159 = DIRECTION ( 'NONE',  ( 0.000000000000000000, -1.000000000000000000, 2.999999999999999839E-15 ) ) ;
#3160 = LINE ( 'NONE', #24791, #12696 ) ;
#3161 = EDGE_CURVE ( 'NONE', #22433, #9537, #7345, .T. ) ;
#3162 = PRODUCT_DEFINITION ( 'UNKNOWN', '', #17057, #4104 ) ;
#3163 = DIRECTION ( 'NONE',  ( -1.734723475976804876E-16, -3.491481338843135327E-15, -1.000000000000000000 ) ) ;
#3164 = ORIENTED_EDGE ( 'NONE', *, *, #14530, .F. ) ;
#3165 = CIRCLE ( 'NONE', #16325, 1.750000000000001554 ) ;
#3166 = ORIENTED_EDGE ( 'NONE', *, *, #10381, .T. ) ;
#3167 = CIRCLE ( 'NONE', #5637, 0.5000000000000004441 ) ;
#3168 = LINE ( 'NONE', #11040, #16121 ) ;
#3169 = DIRECTION ( 'NONE',  ( 0.000000000000000000, 2.999999999999999839E-15, 1.000000000000000000 ) ) ;
#3170 = VECTOR ( 'NONE', #9731, 1000.000000000000000 ) ;
#3171 = VECTOR ( 'NONE', #12539, 1000.000000000000000 ) ;
#3172 = CARTESIAN_POINT ( 'NONE',  ( 39.41296390513587511, -14.41368208888610347, 71.67976084211551324 ) ) ;
#3173 = ORIENTED_EDGE ( 'NONE', *, *, #11868, .F. ) ;
#3174 = ORIENTED_EDGE ( 'NONE', *, *, #22025, .F. ) ;
#3175 = CARTESIAN_POINT ( 'NONE',  ( 32.81606138205700773, 2.476587234117772596, 12.62587505415466538 ) ) ;
#3176 = CARTESIAN_POINT ( 'NONE',  ( 37.69796330110504101, 0.8863179111139003474, 69.66206559358664663 ) ) ;
#3177 = CARTESIAN_POINT ( 'NONE',  ( 38.37017380507018771, -25.60384086642190837, 69.64448340153876416 ) ) ;
#3178 = DIRECTION ( 'NONE',  ( 1.000000000000000000, 1.734723475976805122E-16, -1.734723475976814737E-16 ) ) ;
#3179 = CARTESIAN_POINT ( 'NONE',  ( 36.89935272106204422, -7.213682088886102406, 69.52238214136768590 ) ) ;
#3180 = CARTESIAN_POINT ( 'NONE',  ( 32.81606138205700773, -26.01295748837380373, 65.89261741282676610 ) ) ;
#3181 = ORIENTED_EDGE ( 'NONE', *, *, #23246, .F. ) ;
#3182 = DIRECTION ( 'NONE',  ( 0.9636162972320556630, 0.2672894156317878744, -1.100396788012901859E-15 ) ) ;
#3183 = DIRECTION ( 'NONE',  ( 8.791731484610113542E-17, -0.9135454576426023099, -0.4067366430757970996 ) ) ;
#3184 = CARTESIAN_POINT ( 'NONE',  ( 40.64099152588523367, -1.357181138186998925, 88.30501292736998664 ) ) ;
#3185 = VECTOR ( 'NONE', #8688, 1000.000000000000000 ) ;
#3186 = VECTOR ( 'NONE', #14654, 1000.000000000000000 ) ;
#3187 = FACE_OUTER_BOUND ( 'NONE', #3152, .T. ) ;
#3188 = CARTESIAN_POINT ( 'NONE',  ( 38.26194895904384907, 1.396159133578083633, 73.11602215082119471 ) ) ;
#3189 = DIRECTION ( 'NONE',  ( -1.734723475976804876E-16, -3.491481338843135327E-15, -1.000000000000000000 ) ) ;
#3190 = EDGE_CURVE ( 'NONE', #22354, #4595, #18463, .T. ) ;
#3191 = EDGE_LOOP ( 'NONE', ( #14794, #22561, #441, #24466 ) ) ;
#3192 = DIRECTION ( 'NONE',  ( 1.000000000000000000, 0.000000000000000000, 0.000000000000000000 ) ) ;
#3193 = LINE ( 'NONE', #24443, #13204 ) ;
#3194 = VERTEX_POINT ( 'NONE', #9298 ) ;
#3195 = ORIENTED_EDGE ( 'NONE', *, *, #16006, .F. ) ;
#3196 = CARTESIAN_POINT ( 'NONE',  ( 37.61123632939164452, -17.70384086642190979, 69.02690120949091579 ) ) ;
#3197 = CARTESIAN_POINT ( 'NONE',  ( 37.25202387243752611, -19.21368208888610241, 70.00779233799262613 ) ) ;
#3198 = PLANE ( 'NONE',  #16484 ) ;
#3199 = CIRCLE ( 'NONE', #12271, 1.500000000000000222 ) ;
#3200 = VECTOR ( 'NONE', #4429, 1000.000000000000227 ) ;
#3201 = VECTOR ( 'NONE', #4598, 1000.000000000000000 ) ;
#3202 = EDGE_LOOP ( 'NONE', ( #12001, #23376, #21364, #9011 ) ) ;
#3203 = DIRECTION ( 'NONE',  ( -1.000000000000000000, 0.000000000000000000, 0.000000000000000000 ) ) ;
#3204 = DIRECTION ( 'NONE',  ( 1.000000000000000000, 2.611101091812726599E-15, -1.919289851541777660E-16 ) ) ;
#3205 = EDGE_CURVE ( 'NONE', #848, #2928, #20946, .T. ) ;
#3206 = CARTESIAN_POINT ( 'NONE',  ( 36.07789103942398867, -25.41368208888610525, 70.70992431699450265 ) ) ;
#3207 = ORIENTED_EDGE ( 'NONE', *, *, #7740, .F. ) ;
#3208 = SURFACE_SIDE_STYLE ('',( #7340 ) ) ;
#3209 = CARTESIAN_POINT ( 'NONE',  ( 32.81606138205700773, 35.44123852234597649, 68.30501292736990138 ) ) ;
#3210 = CARTESIAN_POINT ( 'NONE',  ( 38.93415946300897446, -0.1136820888861071466, 73.09843995877331224 ) ) ;
#3211 = CARTESIAN_POINT ( 'NONE',  ( 44.81606138205700063, 39.55420052130484265, 58.58767820587064534 ) ) ;
#3212 = CARTESIAN_POINT ( 'NONE',  ( 36.49096545463212493, -21.51368208888610312, 71.43714994484034264 ) ) ;
#3213 = DIRECTION ( 'NONE',  ( 2.776799322558808202E-15, -0.8967398287344627850, -0.4425581086832400257 ) ) ;
#3214 = CARTESIAN_POINT ( 'NONE',  ( 35.31606138205700773, 7.282926244446937147, 65.60596383066929604 ) ) ;
#3215 = CARTESIAN_POINT ( 'NONE',  ( 37.31647492878124694, -20.30384086642190766, 72.03616607671141026 ) ) ;
#3216 = CARTESIAN_POINT ( 'NONE',  ( 36.64852494920107517, -7.413682088886104360, 70.89533451361948835 ) ) ;
#3217 = VECTOR ( 'NONE', #23669, 1000.000000000000000 ) ;
#3218 = ORIENTED_EDGE ( 'NONE', *, *, #8621, .T. ) ;
#3219 = DIRECTION ( 'NONE',  ( 0.000000000000000000, -1.000000000000000000, 2.999999999999999839E-15 ) ) ;
#3220 = ORIENTED_EDGE ( 'NONE', *, *, #17581, .T. ) ;
#3221 = VECTOR ( 'NONE', #17519, 1000.000000000000000 ) ;
#3222 = CARTESIAN_POINT ( 'NONE',  ( 40.14115730948191185, -7.103840866421910150, 71.43714994484034264 ) ) ;
#3223 = CARTESIAN_POINT ( 'NONE',  ( 46.81606138205696510, -3.028410647649130816, 0.3252050635115383281 ) ) ;
#3224 = CARTESIAN_POINT ( 'NONE',  ( 37.89291511884476904, -27.11368208888610454, 70.26206559358661252 ) ) ;
#3225 = VERTEX_POINT ( 'NONE', #25223 ) ;
#3226 = CARTESIAN_POINT ( 'NONE',  ( 36.98690846071097837, -11.81368208888611093, 73.30173637941818754 ) ) ;
#3227 = ORIENTED_EDGE ( 'NONE', *, *, #22923, .T. ) ;
#3228 = FACE_OUTER_BOUND ( 'NONE', #2278, .T. ) ;
#3229 = CARTESIAN_POINT ( 'NONE',  ( 38.73920764526923932, -13.50384086642191228, 70.26206559358661252 ) ) ;
#3230 = COLOUR_RGB ( '', 0.09019608, 0.27058824, 0.51372549) ;
#3231 = LINE ( 'NONE', #22439, #21691 ) ;
#3232 = VERTEX_POINT ( 'NONE', #21131 ) ;
#3233 = PLANE ( 'NONE',  #23657 ) ;
#3234 = CARTESIAN_POINT ( 'NONE',  ( 34.06606138205700773, -36.11063010576116739, 71.66210679335823386 ) ) ;
#3235 = CARTESIAN_POINT ( 'NONE',  ( 39.02088643472237806, -16.70384086642191690, 73.73360434286898624 ) ) ;
#3236 = CARTESIAN_POINT ( 'NONE',  ( 38.05466885408097255, -22.20914808198024559, 75.80498909504116511 ) ) ;
#3237 = VECTOR ( 'NONE', #3931, 1000.000000000000000 ) ;
#3238 = CARTESIAN_POINT ( 'NONE',  ( 33.56477571746443544, 3.418883076854447367, 6.349191931652266696 ) ) ;
#3239 = CARTESIAN_POINT ( 'NONE',  ( 39.38009889167650357, -20.21368208888610951, 72.75271321436731853 ) ) ;
#3240 = DIRECTION ( 'NONE',  ( -1.000000000000000000, -1.734723475976804876E-16, 1.734723475976814737E-16 ) ) ;
#3241 = DIRECTION ( 'NONE',  ( -1.000000000000000000, 1.115179377413661005E-30, 3.717264591378870232E-16 ) ) ;
#3242 = AXIS2_PLACEMENT_3D ( 'NONE', #3828, #11709, #1259 ) ;
#3243 = ORIENTED_EDGE ( 'NONE', *, *, #15936, .F. ) ;
#3244 = CARTESIAN_POINT ( 'NONE',  ( 33.56606138205700773, -34.55876147765400219, 75.30501292737011454 ) ) ;
#3245 = DIRECTION ( 'NONE',  ( 0.000000000000000000, -0.7540134720837725624, -0.6568589528324736415 ) ) ;
#3246 = CARTESIAN_POINT ( 'NONE',  ( 38.82593461698264292, -8.703840866421913347, 73.13360434286904876 ) ) ;
#3247 = APPLICATION_PROTOCOL_DEFINITION ( 'draft international standard', 'automotive_design', 1998, #10953 ) ;
#3248 = DIRECTION ( 'NONE',  ( 0.000000000000000000, 1.000000000000000000, -2.999999999999999839E-15 ) ) ;
#3249 = AXIS2_PLACEMENT_3D ( 'NONE', #2174, #233, #17915 ) ;
#3250 = EDGE_CURVE ( 'NONE', #8203, #1959, #4071, .T. ) ;
#3251 = CARTESIAN_POINT ( 'NONE',  ( 39.98359781491296161, -26.41368208888610525, 71.86517103874045631 ) ) ;
#3252 = EDGE_CURVE ( 'NONE', #2156, #11682, #22922, .T. ) ;
#3253 = DIRECTION ( 'NONE',  ( 0.000000000000000000, 0.8212051873014210024, 0.5706330172266920187 ) ) ;
#3254 = EDGE_CURVE ( 'NONE', #8848, #4816, #21251, .T. ) ;
#3255 = EDGE_CURVE ( 'NONE', #2367, #6757, #7730, .T. ) ;
#3256 = CARTESIAN_POINT ( 'NONE',  ( 36.68196826583682935, -22.00384086642191406, 70.79240656858107172 ) ) ;
#3257 = ADVANCED_FACE ( 'NONE', ( #7608 ), #3723, .F. ) ;
#3258 = CARTESIAN_POINT ( 'NONE',  ( 36.36697178183959522, -6.686045162182824519, 83.20786762765629874 ) ) ;
#3259 = VECTOR ( 'NONE', #4287, 1000.000000000000000 ) ;
#3260 = CARTESIAN_POINT ( 'NONE',  ( 37.69796330110504101, -19.11368208888610098, 69.66206559358661821 ) ) ;
#3261 = VERTEX_POINT ( 'NONE', #11475 ) ;
#3262 = CARTESIAN_POINT ( 'NONE',  ( 37.61123632939165873, -25.91368208888610880, 73.73360434286898624 ) ) ;
#3263 = VERTEX_POINT ( 'NONE', #3475 ) ;
#3264 = CARTESIAN_POINT ( 'NONE',  ( 39.31606138205700063, 42.19123852234599781, 75.30501292736987295 ) ) ;
#3265 = FACE_OUTER_BOUND ( 'NONE', #16565, .T. ) ;
#3266 = CARTESIAN_POINT ( 'NONE',  ( 37.89291511884476904, 0.8863179111139005695, 70.26206559358665515 ) ) ;
#3267 = VECTOR ( 'NONE', #15116, 1000.000000000000000 ) ;
#3268 = VERTEX_POINT ( 'NONE', #13655 ) ;
#3269 = ORIENTED_EDGE ( 'NONE', *, *, #16792, .T. ) ;
#3270 = CARTESIAN_POINT ( 'NONE',  ( 44.81606138205700063, -22.55876147765401996, 68.80501292737008612 ) ) ;
#3271 = DIRECTION ( 'NONE',  ( 1.000000000000000000, -0.000000000000000000, 0.000000000000000000 ) ) ;
#3272 = ORIENTED_EDGE ( 'NONE', *, *, #8457, .F. ) ;
#3273 = EDGE_CURVE ( 'NONE', #10220, #16812, #5284, .T. ) ;
#3274 = DIRECTION ( 'NONE',  ( -2.690219486203388234E-15, 0.8967398287344627850, 0.4425581086832399147 ) ) ;
#3275 = CARTESIAN_POINT ( 'NONE',  ( 36.49096545463212493, -6.103840866421912814, 71.32335560751963044 ) ) ;
#3276 = EDGE_CURVE ( 'NONE', #9062, #3532, #2415, .T. ) ;
#3277 = CIRCLE ( 'NONE', #369, 3.000000000000002665 ) ;
#3278 = FILL_AREA_STYLE_COLOUR ( '', #16218 ) ;
#3279 = DIRECTION ( 'NONE',  ( -1.956963323498894821E-16, 1.000000000000000000, -2.999999999999999839E-15 ) ) ;
#3280 = ORIENTED_EDGE ( 'NONE', *, *, #9413, .T. ) ;
#3281 = ORIENTED_EDGE ( 'NONE', *, *, #994, .F. ) ;
#3282 = CARTESIAN_POINT ( 'NONE',  ( 45.81606138205700063, -34.55876147765410167, 70.30501292737000085 ) ) ;
#3283 = CARTESIAN_POINT ( 'NONE',  ( 36.87297107704153376, -3.713682088886109511, 72.49904802271743165 ) ) ;
#3284 = EDGE_CURVE ( 'NONE', #25152, #10647, #5413, .T. ) ;
#3285 = DIRECTION ( 'NONE',  ( 0.000000000000000000, 1.000000000000000000, 0.000000000000000000 ) ) ;
#3286 = PLANE ( 'NONE',  #19042 ) ;
#3287 = VECTOR ( 'NONE', #16155, 1000.000000000000000 ) ;
#3288 = ORIENTED_EDGE ( 'NONE', *, *, #22449, .T. ) ;
#3289 = VECTOR ( 'NONE', #2340, 1000.000000000000000 ) ;
#3290 = CARTESIAN_POINT ( 'NONE',  ( 47.81606138205697221, -29.47337283097070326, 44.07055847651734837 ) ) ;
#3291 = CARTESIAN_POINT ( 'NONE',  ( 39.81606138205700063, -4.399276463885007260, 59.51717649063222382 ) ) ;
#3292 = VECTOR ( 'NONE', #676, 1000.000000000000000 ) ;
#3293 = CYLINDRICAL_SURFACE ( 'NONE', #19734, 1.000000000000000888 ) ;
#3294 = FACE_OUTER_BOUND ( 'NONE', #4552, .T. ) ;
#3295 =( NAMED_UNIT ( * ) PLANE_ANGLE_UNIT ( ) SI_UNIT ( $, .RADIAN. ) );
#3296 = VERTEX_POINT ( 'NONE', #1526 ) ;
#3297 = AXIS2_PLACEMENT_3D ( 'NONE', #10319, #507, #8394 ) ;
#3298 = CARTESIAN_POINT ( 'NONE',  ( 40.31606138205700773, -31.05876147765400574, 73.55501292737010033 ) ) ;
#3299 = ORIENTED_EDGE ( 'NONE', *, *, #16653, .T. ) ;
#3300 = VERTEX_POINT ( 'NONE', #11222 ) ;
#3301 = DIRECTION ( 'NONE',  ( 0.000000000000000000, 1.000000000000000000, 0.000000000000000000 ) ) ;
#3302 = DIRECTION ( 'NONE',  ( 0.000000000000000000, -0.4425581086832348077, 0.8967398287344653385 ) ) ;
#3303 = CARTESIAN_POINT ( 'NONE',  ( 37.25260217561390874, -19.61368208888610098, 71.78268878715392987 ) ) ;
#3304 = ORIENTED_EDGE ( 'NONE', *, *, #20261, .T. ) ;
#3305 = ORIENTED_EDGE ( 'NONE', *, *, #5617, .T. ) ;
#3306 = DIRECTION ( 'NONE',  ( 0.000000000000000000, -1.000000000000000000, 4.163336342344336238E-15 ) ) ;
#3307 = PLANE ( 'NONE',  #11587 ) ;
#3308 = CARTESIAN_POINT ( 'NONE',  ( 37.33957961208645315, -21.80384086642190766, 69.94417936956672577 ) ) ;
#3309 = CIRCLE ( 'NONE', #4127, 1.250000000000000888 ) ;
#3310 = CARTESIAN_POINT ( 'NONE',  ( 42.99807726499842175, 2.836257474661138644, 6.100376100592989737 ) ) ;
#3311 = CARTESIAN_POINT ( 'NONE',  ( 36.07789103942398867, -3.413682088886104804, 70.70992431699450265 ) ) ;
#3312 = VERTEX_POINT ( 'NONE', #19316 ) ;
#3313 = VECTOR ( 'NONE', #7589, 1000.000000000000000 ) ;
#3314 = VERTEX_POINT ( 'NONE', #19072 ) ;
#3315 = DIRECTION ( 'NONE',  ( -0.000000000000000000, -3.469446951953613400E-15, -1.000000000000000000 ) ) ;
#3316 = ADVANCED_FACE ( 'NONE', ( #21378 ), #13279, .F. ) ;
#3317 = EDGE_CURVE ( 'NONE', #16994, #4665, #1649, .T. ) ;
#3318 = DIRECTION ( 'NONE',  ( 0.000000000000000000, 0.7540134720837716742, 0.6568589528324746407 ) ) ;
#3319 = CARTESIAN_POINT ( 'NONE',  ( 35.91606138205694521, 3.586515973360777654, -0.5067327973472466329 ) ) ;
#3320 = CARTESIAN_POINT ( 'NONE',  ( 38.96303889229209716, -5.307263880975074066, 83.30967742110996710 ) ) ;
#3321 = DIRECTION ( 'NONE',  ( -2.290324355028189071E-16, 0.4067366430757970996, -0.9135454576426023099 ) ) ;
#3322 = CARTESIAN_POINT ( 'NONE',  ( 38.31606138205700063, -7.415330352220093069, 56.88974067930232081 ) ) ;
#3323 = ORIENTED_EDGE ( 'NONE', *, *, #1674, .T. ) ;
#3324 = FACE_OUTER_BOUND ( 'NONE', #652, .T. ) ;
#3325 = DIRECTION ( 'NONE',  ( -1.000000000000000000, -2.999999999999999839E-15, 0.000000000000000000 ) ) ;
#3326 = ORIENTED_EDGE ( 'NONE', *, *, #7846, .T. ) ;
#3327 = EDGE_LOOP ( 'NONE', ( #12452, #6895, #16216, #13853 ) ) ;
#3328 = UNCERTAINTY_MEASURE_WITH_UNIT (LENGTH_MEASURE( 1.000000000000000082E-05 ), #4972, 'distance_accuracy_value', 'NONE');
#3329 = VECTOR ( 'NONE', #7940, 1000.000000000000000 ) ;
#3330 = CARTESIAN_POINT ( 'NONE',  ( 39.12911128074872380, -11.50384086642191050, 69.06206559358666652 ) ) ;
#3331 = LINE ( 'NONE', #5532, #19828 ) ;
#3332 = CARTESIAN_POINT ( 'NONE',  ( 39.98359781491296161, -24.41368208888610525, 71.86517103874045631 ) ) ;
#3333 =( LENGTH_UNIT ( ) NAMED_UNIT ( * ) SI_UNIT ( .MILLI., .METRE. ) );
#3334 = ORIENTED_EDGE ( 'NONE', *, *, #8960, .T. ) ;
#3335 = DIRECTION ( 'NONE',  ( -1.849283715844614456E-16, 0.8212051873014208914, 0.5706330172266919076 ) ) ;
#3336 = DIRECTION ( 'NONE',  ( -1.000000000000000000, 0.000000000000000000, 0.000000000000000000 ) ) ;
#3337 = CARTESIAN_POINT ( 'NONE',  ( 35.86008812008917346, -19.51368208888610312, 71.43714994484034264 ) ) ;
#3338 = ORIENTED_EDGE ( 'NONE', *, *, #21854, .F. ) ;
#3339 = EDGE_CURVE ( 'NONE', #12061, #126, #5720, .T. ) ;
#3340 = DIRECTION ( 'NONE',  ( -2.122643018205887308E-17, 1.000000000000000000, -3.120611096041553009E-15 ) ) ;
#3341 = EDGE_CURVE ( 'NONE', #4343, #20215, #16083, .T. ) ;
#3342 = CARTESIAN_POINT ( 'NONE',  ( 39.29254315202756231, 1.186317911113898838, 69.94417936956675419 ) ) ;
#3343 = FACE_OUTER_BOUND ( 'NONE', #3702, .T. ) ;
#3344 = CARTESIAN_POINT ( 'NONE',  ( 39.98359781491296161, -14.41368208888610525, 71.86517103874047052 ) ) ;
#3345 = CIRCLE ( 'NONE', #19383, 0.5000000000000004441 ) ;
#3346 = DIRECTION ( 'NONE',  ( 1.000000000000000000, 0.000000000000000000, 0.000000000000000000 ) ) ;
#3347 = AXIS2_PLACEMENT_3D ( 'NONE', #20363, #2315, #379 ) ;
#3348 = DIRECTION ( 'NONE',  ( 1.734723475976804876E-16, 3.469446951953610245E-15, 1.000000000000000000 ) ) ;
#3349 = CARTESIAN_POINT ( 'NONE',  ( 38.73920764526923932, -21.50384086642191406, 70.26206559358661252 ) ) ;
#3350 = CARTESIAN_POINT ( 'NONE',  ( 38.37017380507020192, -8.013682088886108446, 73.11602215082118050 ) ) ;
#3351 = EDGE_LOOP ( 'NONE', ( #7734, #12715, #5817, #24669 ) ) ;
#3352 = DIRECTION ( 'NONE',  ( 0.000000000000000000, -0.8212051873014252212, -0.5706330172266858014 ) ) ;
#3353 = EDGE_CURVE ( 'NONE', #17400, #19611, #1181, .T. ) ;
#3354 = CARTESIAN_POINT ( 'NONE',  ( 39.81746892067405952, 42.57231754924293909, 79.37823623207320622 ) ) ;
#3355 = ORIENTED_EDGE ( 'NONE', *, *, #9648, .T. ) ;
#3356 = EDGE_LOOP ( 'NONE', ( #23510, #24602, #16175, #23690 ) ) ;
#3357 = CARTESIAN_POINT ( 'NONE',  ( 37.69796330110505522, -8.503840866421915834, 73.09843995877331224 ) ) ;
#3358 = CARTESIAN_POINT ( 'NONE',  ( 33.31606138205697931, -6.570990706613088150, -2.335727660491067503 ) ) ;
#3359 = CARTESIAN_POINT ( 'NONE',  ( 39.98359781491296161, -0.4136820888861053591, 71.86517103874048473 ) ) ;
#3360 = EDGE_LOOP ( 'NONE', ( #15024, #19497, #9144, #3504 ) ) ;
#3361 = CARTESIAN_POINT ( 'NONE',  ( 40.33642880535524000, -6.313682088886107380, 72.77780686321128201 ) ) ;
#3362 = ORIENTED_EDGE ( 'NONE', *, *, #7097, .F. ) ;
#3363 = CARTESIAN_POINT ( 'NONE',  ( 33.31606138205700773, -11.22674583108233115, 81.40610939240433197 ) ) ;
#3364 = VECTOR ( 'NONE', #12666, 1000.000000000000000 ) ;
#3365 = CARTESIAN_POINT ( 'NONE',  ( 39.02742774030101458, -7.403840866421910860, 70.49320253461759478 ) ) ;
#3366 = FACE_OUTER_BOUND ( 'NONE', #13790, .T. ) ;
#3367 = EDGE_LOOP ( 'NONE', ( #25040, #9996, #22376, #20015 ) ) ;
#3368 = DIRECTION ( 'NONE',  ( -1.734723475976804876E-16, 1.000000000000000000, 0.000000000000000000 ) ) ;
#3369 = LINE ( 'NONE', #1171, #6711 ) ;
#3370 = AXIS2_PLACEMENT_3D ( 'NONE', #9033, #24457, #6829 ) ;
#3371 = CARTESIAN_POINT ( 'NONE',  ( 40.52078840805429394, -9.003840866421915834, 72.15350918040385864 ) ) ;
#3372 = CARTESIAN_POINT ( 'NONE',  ( 36.51558096900348005, -21.10182828056061055, 75.36712134771262583 ) ) ;
#3373 = SURFACE_STYLE_FILL_AREA ( #8812 ) ;
#3374 = CARTESIAN_POINT ( 'NONE',  ( 37.80618814713140097, -19.91368208888610170, 73.13360434286903455 ) ) ;
#3375 = CARTESIAN_POINT ( 'NONE',  ( 33.31606138205700773, -11.22674583108233115, 81.40610939240433197 ) ) ;
#3376 = CARTESIAN_POINT ( 'NONE',  ( 31.81606138205700418, 40.34464305740947054, 81.44836866983821722 ) ) ;
#3377 = VERTEX_POINT ( 'NONE', #2545 ) ;
#3378 = FACE_OUTER_BOUND ( 'NONE', #3000, .T. ) ;
#3379 = LINE ( 'NONE', #14595, #15106 ) ;
#3380 = CIRCLE ( 'NONE', #10783, 1.750000000000001554 ) ;
#3381 = CARTESIAN_POINT ( 'NONE',  ( 40.14115730948191185, -9.103840866421911926, 71.43714994484034264 ) ) ;
#3382 = PRODUCT_CONTEXT ( 'NONE', #16546, 'mechanical' ) ;
#3383 = LINE ( 'NONE', #20914, #20316 ) ;
#3384 = CARTESIAN_POINT ( 'NONE',  ( 37.25202387243752611, -23.21368208888610241, 70.00779233799262613 ) ) ;
#3385 = CARTESIAN_POINT ( 'NONE',  ( 33.81606138205700063, 2.191238522347003226, 70.30501292737000085 ) ) ;
#3386 = ADVANCED_FACE ( 'NONE', ( #23808 ), #9923, .T. ) ;
#3387 = VECTOR ( 'NONE', #13615, 1000.000000000000000 ) ;
#3388 = CARTESIAN_POINT ( 'NONE',  ( 40.14115730948191185, -27.10384086642190482, 71.43714994484028580 ) ) ;
#3389 = DIRECTION ( 'NONE',  ( 0.000000000000000000, -0.7540134720837687876, -0.6568589528324780824 ) ) ;
#3390 = VECTOR ( 'NONE', #7193, 1000.000000000000000 ) ;
#3391 = CARTESIAN_POINT ( 'NONE',  ( 39.75915168707250302, -16.71368208888609885, 70.26145752964251301 ) ) ;
#3392 = EDGE_LOOP ( 'NONE', ( #19337, #18765, #10376, #22222 ) ) ;
#3393 = CARTESIAN_POINT ( 'NONE',  ( 36.89935272106204422, -27.21368208888609885, 69.52238214136765748 ) ) ;
#3394 = CIRCLE ( 'NONE', #21099, 0.2000000000000057288 ) ;
#3395 = VERTEX_POINT ( 'NONE', #20080 ) ;
#3396 = DIRECTION ( 'NONE',  ( 0.000000000000000000, 0.5706330172266920187, -0.8212051873014210024 ) ) ;
#3397 = CARTESIAN_POINT ( 'NONE',  ( 43.06606138205700063, 41.44123852234599070, 73.55501292736987295 ) ) ;
#3398 = CARTESIAN_POINT ( 'NONE',  ( 37.60469502381300799, -26.40384086642190908, 72.26730301774232146 ) ) ;
#3399 = EDGE_LOOP ( 'NONE', ( #3784, #21354, #17130, #15149 ) ) ;
#3400 = VERTEX_POINT ( 'NONE', #5923 ) ;
#3401 = CARTESIAN_POINT ( 'NONE',  ( 40.31606138205701484, -21.38339321089542011, 27.67811916372966863 ) ) ;
#3402 = DIRECTION ( 'NONE',  ( -1.000000000000000000, -1.000000000000000078E-15, 0.000000000000000000 ) ) ;
#3403 = ORIENTED_EDGE ( 'NONE', *, *, #14691, .F. ) ;
#3404 =( NAMED_UNIT ( * ) SI_UNIT ( $, .STERADIAN. ) SOLID_ANGLE_UNIT ( ) );
#3405 = CARTESIAN_POINT ( 'NONE',  ( 40.14115730948191185, -7.103840866421910150, 71.43714994484034264 ) ) ;
#3406 = AXIS2_PLACEMENT_3D ( 'NONE', #19803, #2765, #3154 ) ;
#3407 = EDGE_CURVE ( 'NONE', #2216, #7931, #18892, .T. ) ;
#3408 = CARTESIAN_POINT ( 'NONE',  ( 30.81606138205700773, 34.87886987267149408, 81.44836866983821722 ) ) ;
#3409 = ADVANCED_FACE ( 'NONE', ( #12370 ), #2044, .F. ) ;
#3410 = DIRECTION ( 'NONE',  ( -1.000000000000000000, 0.000000000000000000, 0.000000000000000000 ) ) ;
#3411 = EDGE_LOOP ( 'NONE', ( #23488, #7531, #177, #14835 ) ) ;
#3412 = EDGE_CURVE ( 'NONE', #17256, #9754, #23558, .T. ) ;
#3413 = EDGE_LOOP ( 'NONE', ( #19615, #17036, #3971, #3094 ) ) ;
#3414 = LINE ( 'NONE', #13088, #956 ) ;
#3415 = CARTESIAN_POINT ( 'NONE',  ( 38.82593461698262871, -0.9136820888861021395, 69.62690120949091011 ) ) ;
#3416 = VECTOR ( 'NONE', #8746, 1000.000000000000000 ) ;
#3417 = CARTESIAN_POINT ( 'NONE',  ( 39.29254315202757653, -24.80384086642191477, 72.81632618279320468 ) ) ;
#3418 = LINE ( 'NONE', #9361, #12475 ) ;
#3419 = ORIENTED_EDGE ( 'NONE', *, *, #18856, .T. ) ;
#3420 = LINE ( 'NONE', #15017, #22147 ) ;
#3421 = EDGE_CURVE ( 'NONE', #16162, #19839, #2421, .T. ) ;
#3422 = CIRCLE ( 'NONE', #6705, 1.000000000000000888 ) ;
#3423 = AXIS2_PLACEMENT_3D ( 'NONE', #16922, #12809, #1060 ) ;
#3424 = LINE ( 'NONE', #17090, #22197 ) ;
#3425 = DIRECTION ( 'NONE',  ( 0.000000000000000000, 2.999999999999999839E-15, 1.000000000000000000 ) ) ;
#3426 =( NAMED_UNIT ( * ) PLANE_ANGLE_UNIT ( ) SI_UNIT ( $, .RADIAN. ) );
#3427 = ORIENTED_EDGE ( 'NONE', *, *, #19047, .F. ) ;
#3428 = VECTOR ( 'NONE', #14336, 1000.000000000000000 ) ;
#3429 = LINE ( 'NONE', #25165, #3725 ) ;
#3430 = ORIENTED_EDGE ( 'NONE', *, *, #6322, .F. ) ;
#3431 = VERTEX_POINT ( 'NONE', #17780 ) ;
#3432 = CARTESIAN_POINT ( 'NONE',  ( 43.62725655850141493, 3.386289273678555922, 6.178516409519463792 ) ) ;
#3433 = CARTESIAN_POINT ( 'NONE',  ( 40.31606138205697931, -5.528433326023618477, -4.448224773462933435 ) ) ;
#3434 = CARTESIAN_POINT ( 'NONE',  ( 38.73920764526925353, -8.113682088886099208, 72.49843995877331793 ) ) ;
#3435 = VERTEX_POINT ( 'NONE', #19960 ) ;
#3436 = VECTOR ( 'NONE', #14093, 1000.000000000000227 ) ;
#3437 = ORIENTED_EDGE ( 'NONE', *, *, #7893, .T. ) ;
#3438 = PLANE ( 'NONE',  #4644 ) ;
#3439 = CARTESIAN_POINT ( 'NONE',  ( 36.81465384343994884, 40.76768529863396395, 79.37823623207322044 ) ) ;
#3440 = CARTESIAN_POINT ( 'NONE',  ( 36.68196826583682935, -26.00384086642191406, 70.79240656858105751 ) ) ;
#3441 = COLOUR_RGB ( '', 0.09019608, 0.27058824, 0.51372549) ;
#3442 = EDGE_CURVE ( 'NONE', #58, #1644, #2294, .T. ) ;
#3443 = LINE ( 'NONE', #9262, #8327 ) ;
#3444 = AXIS2_PLACEMENT_3D ( 'NONE', #19832, #8112, #10052 ) ;
#3445 = EDGE_CURVE ( 'NONE', #7878, #14092, #9043, .T. ) ;
#3446 = EDGE_CURVE ( 'NONE', #14751, #24251, #107, .T. ) ;
#3447 = CARTESIAN_POINT ( 'NONE',  ( 43.06468080341933558, 3.415100481988189607, 6.350457055188961419 ) ) ;
#3448 = AXIS2_PLACEMENT_3D ( 'NONE', #19213, #15732, #23195 ) ;
#3449 = LINE ( 'NONE', #13494, #11858 ) ;
#3450 = DIRECTION ( 'NONE',  ( 0.000000000000000000, 4.476705744456288765E-15, 1.000000000000000000 ) ) ;
#3451 = CARTESIAN_POINT ( 'NONE',  ( 39.54057891361352972, -5.617563030284176584, 83.30218584522116032 ) ) ;
#3452 = LINE ( 'NONE', #13629, #9000 ) ;
#3453 = EDGE_CURVE ( 'NONE', #21357, #19154, #11862, .T. ) ;
#3454 = DIRECTION ( 'NONE',  ( 0.000000000000000000, 0.6568589528324746407, -0.7540134720837717852 ) ) ;
#3455 = EDGE_LOOP ( 'NONE', ( #580, #12966, #3011, #22594 ) ) ;
#3456 = LINE ( 'NONE', #24558, #11519 ) ;
#3457 = DIRECTION ( 'NONE',  ( 0.000000000000000000, 0.7540134720837717852, 0.6568589528324746407 ) ) ;
#3458 = ORIENTED_EDGE ( 'NONE', *, *, #25191, .F. ) ;
#3459 = ORIENTED_EDGE ( 'NONE', *, *, #7029, .F. ) ;
#3460 = CARTESIAN_POINT ( 'NONE',  ( 39.73277004305197124, -11.40384086642191086, 69.52238214136768590 ) ) ;
#3461 = ADVANCED_FACE ( 'NONE', ( #8369 ), #19830, .T. ) ;
#3462 = AXIS2_PLACEMENT_3D ( 'NONE', #11467, #19304, #1774 ) ;
#3463 = LINE ( 'NONE', #6724, #9559 ) ;
#3464 = CARTESIAN_POINT ( 'NONE',  ( 38.37017380507020192, -14.01368208888610845, 73.11602215082116629 ) ) ;
#3465 = FILL_AREA_STYLE ('',( #17378 ) ) ;
#3466 = VERTEX_POINT ( 'NONE', #15831 ) ;
#3467 = CARTESIAN_POINT ( 'NONE',  ( 41.31606138205687273, 33.19123852234595518, 61.30501292736990848 ) ) ;
#3468 = DIRECTION ( 'NONE',  ( 0.000000000000000000, 1.000000000000000000, 0.000000000000000000 ) ) ;
#3469 = CARTESIAN_POINT ( 'NONE',  ( 36.11133435605973574, -21.61368208888610454, 72.15350918040385864 ) ) ;
#3470 = ORIENTED_EDGE ( 'NONE', *, *, #9002, .F. ) ;
#3471 = AXIS2_PLACEMENT_3D ( 'NONE', #6614, #14597, #10620 ) ;
#3472 = DIRECTION ( 'NONE',  ( 1.734723475976804876E-16, 3.491481338843135327E-15, 1.000000000000000000 ) ) ;
#3473 = PLANE ( 'NONE',  #18226 ) ;
#3474 = AXIS2_PLACEMENT_3D ( 'NONE', #7406, #20807, #21185 ) ;
#3475 = CARTESIAN_POINT ( 'NONE',  ( 41.32070064951228971, -37.35828293338759920, 83.30501292737011454 ) ) ;
#3476 = CARTESIAN_POINT ( 'NONE',  ( 36.31606138205700063, -7.204193249396275256, 83.11277699141410835 ) ) ;
#3477 = CARTESIAN_POINT ( 'NONE',  ( 38.73920764526923932, -13.50384086642191228, 70.26206559358661252 ) ) ;
#3478 = CARTESIAN_POINT ( 'NONE',  ( 39.98359781491296161, -0.4136820888861053591, 71.86517103874048473 ) ) ;
#3479 = ORIENTED_EDGE ( 'NONE', *, *, #17709, .F. ) ;
#3480 = LINE ( 'NONE', #1420, #359 ) ;
#3481 = LINE ( 'NONE', #16399, #18524 ) ;
#3482 = ORIENTED_EDGE ( 'NONE', *, *, #13193, .T. ) ;
#3483 = VERTEX_POINT ( 'NONE', #6051 ) ;
#3484 = EDGE_CURVE ( 'NONE', #21718, #23642, #13907, .T. ) ;
#3485 = CARTESIAN_POINT ( 'NONE',  ( 36.36258059203030513, -27.90384086642191264, 69.89063713639258424 ) ) ;
#3486 = EDGE_CURVE ( 'NONE', #21683, #5803, #615, .T. ) ;
#3487 = EDGE_CURVE ( 'NONE', #4816, #16043, #2171, .T. ) ;
#3488 = CARTESIAN_POINT ( 'NONE',  ( 38.26194895904383486, 0.9863179111138999922, 69.64448340153880679 ) ) ;
#3489 = CARTESIAN_POINT ( 'NONE',  ( 40.77203464402485622, -2.513682088886103116, 71.32335560751961623 ) ) ;
#3490 = ORIENTED_EDGE ( 'NONE', *, *, #19731, .F. ) ;
#3491 = DIRECTION ( 'NONE',  ( -2.011972697750612571E-15, 0.6595716529892353686, -0.7516416929448815898 ) ) ;
#3492 = CARTESIAN_POINT ( 'NONE',  ( 38.00113996487112189, -3.703840866421909794, 70.22690120949091863 ) ) ;
#3493 = SURFACE_STYLE_FILL_AREA ( #19094 ) ;
#3494 = ORIENTED_EDGE ( 'NONE', *, *, #20044, .F. ) ;
#3495 = FACE_OUTER_BOUND ( 'NONE', #2062, .T. ) ;
#3496 = DIRECTION ( 'NONE',  ( 1.000000000000000000, 0.000000000000000000, 0.000000000000000000 ) ) ;
#3497 = CARTESIAN_POINT ( 'NONE',  ( 40.52078840805429394, -7.003840866421914058, 72.15350918040385864 ) ) ;
#3498 = CARTESIAN_POINT ( 'NONE',  ( 38.31606138205700063, -22.22127907754186893, 75.29996292736998953 ) ) ;
#3499 = PRESENTATION_STYLE_ASSIGNMENT (( #137 ) ) ;
#3500 = CARTESIAN_POINT ( 'NONE',  ( 38.26194895904383486, -15.01368208888610134, 69.64448340153877837 ) ) ;
#3501 = DIRECTION ( 'NONE',  ( -1.000000000000000000, -1.734723475976804876E-16, 1.734723475976814737E-16 ) ) ;
#3502 = EDGE_CURVE ( 'NONE', #25135, #22767, #14035, .T. ) ;
#3503 = DIRECTION ( 'NONE',  ( -1.000000000000000000, 0.000000000000000000, 0.000000000000000000 ) ) ;
#3504 = ORIENTED_EDGE ( 'NONE', *, *, #16814, .F. ) ;
#3505 = CARTESIAN_POINT ( 'NONE',  ( 44.71606138205695657, 0.5799492015812843793, -3.145019409304214530 ) ) ;
#3506 = CARTESIAN_POINT ( 'NONE',  ( 37.33957961208645315, -5.803840866421907663, 69.94417936956673998 ) ) ;
#3507 = VECTOR ( 'NONE', #24321, 1000.000000000000000 ) ;
#3508 = APPLICATION_PROTOCOL_DEFINITION ( 'draft international standard', 'automotive_design', 1998, #1713 ) ;
#3509 = CARTESIAN_POINT ( 'NONE',  ( 42.81606138205700063, 22.19123852234699967, 69.30501292736994401 ) ) ;
#3510 = CARTESIAN_POINT ( 'NONE',  ( 39.38009889167650357, -16.21368208888610596, 72.75271321436731853 ) ) ;
#3511 = LINE ( 'NONE', #11385, #10243 ) ;
#3512 = CARTESIAN_POINT ( 'NONE',  ( 37.69796330110505522, -16.50384086642191761, 73.09843995877329803 ) ) ;
#3513 = CARTESIAN_POINT ( 'NONE',  ( 37.42710149357921523, -5.398092219773776179, 82.80324863345541075 ) ) ;
#3514 = CARTESIAN_POINT ( 'NONE',  ( 39.95015449827720744, -16.61368208888610454, 70.79240656858105751 ) ) ;
#3515 = ORIENTED_EDGE ( 'NONE', *, *, #23388, .T. ) ;
#3516 = CARTESIAN_POINT ( 'NONE',  ( 37.61123632939165873, -27.91368208888610880, 73.73360434286898624 ) ) ;
#3517 = ORIENTED_EDGE ( 'NONE', *, *, #24069, .F. ) ;
#3518 = DIRECTION ( 'NONE',  ( 1.734723475976804876E-16, 3.491481338843135327E-15, 1.000000000000000000 ) ) ;
#3519 = CARTESIAN_POINT ( 'NONE',  ( 43.31606138205700063, -3.566646240838321269, 18.16837712155798457 ) ) ;
#3520 = CARTESIAN_POINT ( 'NONE',  ( 37.31647492878124694, -22.30384086642191122, 72.03616607671141026 ) ) ;
#3521 = ORIENTED_EDGE ( 'NONE', *, *, #5510, .T. ) ;
#3522 = ORIENTED_EDGE ( 'NONE', *, *, #2038, .F. ) ;
#3523 = DIRECTION ( 'NONE',  ( 0.000000000000000000, 0.7540134720837716742, 0.6568589528324746407 ) ) ;
#3524 = CARTESIAN_POINT ( 'NONE',  ( 39.81746892067405952, 42.57231754924293909, 79.57823623207322328 ) ) ;
#3525 = ORIENTED_EDGE ( 'NONE', *, *, #18398, .T. ) ;
#3526 = CARTESIAN_POINT ( 'NONE',  ( 30.81606138205694378, 5.290470704224592424, -0.3848988112044732235 ) ) ;
#3527 = CARTESIAN_POINT ( 'NONE',  ( 39.02088643472237806, -26.70384086642192401, 73.73360434286898624 ) ) ;
#3528 = CARTESIAN_POINT ( 'NONE',  ( 36.31606138205700773, -23.16691978223482096, 31.29201591705069063 ) ) ;
#3529 = EDGE_CURVE ( 'NONE', #14213, #21871, #21890, .T. ) ;
#3530 = B_SPLINE_SURFACE_WITH_KNOTS ( 'NONE', 1, 3, ( 
 ( #1467, #18868, #7017, #17192 ),
 ( #14865, #25018, #11283, #22727 ),
 ( #1207, #9095, #16937, #13078 ) ),
 .UNSPECIFIED., .F., .F., .F.,
 ( 2, 1, 2 ),
 ( 4, 4 ),
 ( -0.01000000000000000021, 0.000000000000000000, 1.000000000000000000 ),
 ( 0.000000000000000000, 1.000000000000000000 ),
 .UNSPECIFIED. ) ;
#3531 = LINE ( 'NONE', #11405, #13900 ) ;
#3532 = VERTEX_POINT ( 'NONE', #12998 ) ;
#3533 = ORIENTED_EDGE ( 'NONE', *, *, #9274, .T. ) ;
#3534 = DIRECTION ( 'NONE',  ( 0.000000000000000000, -1.000000000000000000, 0.000000000000000000 ) ) ;
#3535 = LINE ( 'NONE', #5478, #22502 ) ;
#3536 = CARTESIAN_POINT ( 'NONE',  ( 38.26194895904384907, -24.60384086642191548, 73.11602215082115208 ) ) ;
#3537 =( NAMED_UNIT ( * ) PLANE_ANGLE_UNIT ( ) SI_UNIT ( $, .RADIAN. ) );
#3538 = CARTESIAN_POINT ( 'NONE',  ( 45.81606138205707168, -36.80651332587431313, 65.82119181171029254 ) ) ;
#3539 = ORIENTED_EDGE ( 'NONE', *, *, #20763, .F. ) ;
#3540 = CARTESIAN_POINT ( 'NONE',  ( 42.81606138205700063, 2.191238522347013884, 73.80501292737000085 ) ) ;
#3541 = CARTESIAN_POINT ( 'NONE',  ( 31.81606138205700418, -34.55876147765400930, 73.30501292737011454 ) ) ;
#3542 = FACE_OUTER_BOUND ( 'NONE', #19197, .T. ) ;
#3543 =( LENGTH_UNIT ( ) NAMED_UNIT ( * ) SI_UNIT ( .MILLI., .METRE. ) );
#3544 = ORIENTED_EDGE ( 'NONE', *, *, #32, .F. ) ;
#3545 = PLANE ( 'NONE',  #426 ) ;
#3546 = ORIENTED_EDGE ( 'NONE', *, *, #13010, .F. ) ;
#3547 = ORIENTED_EDGE ( 'NONE', *, *, #9413, .F. ) ;
#3548 = DIRECTION ( 'NONE',  ( 9.925461516413211857E-16, -0.8967398287344598984, -0.4425581086832454658 ) ) ;
#3549 = CARTESIAN_POINT ( 'NONE',  ( 37.38336156205274818, -9.713682088886098853, 72.12822762946751709 ) ) ;
#3550 = CARTESIAN_POINT ( 'NONE',  ( 39.37952058850012804, -10.61368208888610276, 70.97781676520601479 ) ) ;
#3551 = ORIENTED_EDGE ( 'NONE', *, *, #14599, .F. ) ;
#3552 = ORIENTED_EDGE ( 'NONE', *, *, #1378, .F. ) ;
#3553 = CARTESIAN_POINT ( 'NONE',  ( 31.81606138205700418, 24.50429740018177682, 101.9912164131601457 ) ) ;
#3554 = ORIENTED_EDGE ( 'NONE', *, *, #13651, .T. ) ;
#3555 = FACE_OUTER_BOUND ( 'NONE', #11528, .T. ) ;
#3556 = CARTESIAN_POINT ( 'NONE',  ( 39.95015449827720744, -17.00384086642191406, 71.96809898377887293 ) ) ;
#3557 = CARTESIAN_POINT ( 'NONE',  ( 42.82505858241695762, 3.225987868298963779, 6.370930886792723236 ) ) ;
#3558 = ADVANCED_FACE ( 'NONE', ( #3187 ), #12004, .T. ) ;
#3559 = CARTESIAN_POINT ( 'NONE',  ( 38.73920764526925353, -16.11368208888610454, 72.49843995877330372 ) ) ;
#3560 = CARTESIAN_POINT ( 'NONE',  ( 45.81606138205700063, -33.05876147765410167, 70.30501292737000085 ) ) ;
#3561 = CARTESIAN_POINT ( 'NONE',  ( 30.81606138205707168, -37.26069504592557990, 64.48189387429259511 ) ) ;
#3562 = DIRECTION ( 'NONE',  ( -1.000000000000000000, -2.999999999999999839E-15, 0.000000000000000000 ) ) ;
#3563 = CARTESIAN_POINT ( 'NONE',  ( 39.32110845963273960, -5.470149936707826122, 83.30695469465730696 ) ) ;
#3564 = DIRECTION ( 'NONE',  ( 0.000000000000000000, 0.1918498038142812112, -0.9814242980364923374 ) ) ;
#3565 = AXIS2_PLACEMENT_3D ( 'NONE', #1856, #23499, #13357 ) ;
#3566 = CARTESIAN_POINT ( 'NONE',  ( 38.31606138205700063, -6.549308025893449070, 20.35783565644092619 ) ) ;
#3567 = EDGE_CURVE ( 'NONE', #11430, #8412, #21363, .T. ) ;
#3568 = VECTOR ( 'NONE', #24239, 1000.000000000000000 ) ;
#3569 = AXIS2_PLACEMENT_3D ( 'NONE', #6497, #7937, #4190 ) ;
#3570 = ORIENTED_EDGE ( 'NONE', *, *, #22873, .T. ) ;
#3571 = EDGE_CURVE ( 'NONE', #11586, #20804, #22520, .T. ) ;
#3572 = DIRECTION ( 'NONE',  ( 0.000000000000000000, 1.000000000000000000, 0.000000000000000000 ) ) ;
#3573 = DIRECTION ( 'NONE',  ( 1.000000000000000000, 2.751104698760144965E-15, -1.228345504986737969E-16 ) ) ;
#3574 = ORIENTED_EDGE ( 'NONE', *, *, #16965, .F. ) ;
#3575 = ADVANCED_FACE ( 'NONE', ( #18412 ), #6675, .F. ) ;
#3576 = ORIENTED_EDGE ( 'NONE', *, *, #16976, .T. ) ;
#3577 = CARTESIAN_POINT ( 'NONE',  ( 37.61123632939164452, -9.703840866421911571, 69.02690120949094421 ) ) ;
#3578 = EDGE_CURVE ( 'NONE', #19784, #11454, #16590, .T. ) ;
#3579 = FACE_OUTER_BOUND ( 'NONE', #2632, .T. ) ;
#3580 = CARTESIAN_POINT ( 'NONE',  ( 37.25202387243752611, -15.21368208888610063, 70.00779233799262613 ) ) ;
#3581 = ORIENTED_EDGE ( 'NONE', *, *, #5626, .F. ) ;
#3582 = CARTESIAN_POINT ( 'NONE',  ( 44.81606138205700063, -21.15876147765404625, 76.30501292736998664 ) ) ;
#3583 = CARTESIAN_POINT ( 'NONE',  ( 43.81606138205700063, 2.191238522347000117, 69.30501292737000085 ) ) ;
#3584 = EDGE_CURVE ( 'NONE', #13207, #10501, #2799, .T. ) ;
#3585 = CARTESIAN_POINT ( 'NONE',  ( 36.98690846071097837, -19.81368208888611093, 73.30173637941818754 ) ) ;
#3586 = AXIS2_PLACEMENT_3D ( 'NONE', #14833, #7241, #6984 ) ;
#3587 = ADVANCED_FACE ( 'NONE', ( #8496, #22265 ), #10685, .T. ) ;
#3588 = ORIENTED_EDGE ( 'NONE', *, *, #3273, .F. ) ;
#3589 = CARTESIAN_POINT ( 'NONE',  ( 35.56606138205702194, -20.30191568716149675, 23.22716926412510219 ) ) ;
#3590 = VECTOR ( 'NONE', #21544, 1000.000000000000000 ) ;
#3591 = CIRCLE ( 'NONE', #15935, 0.7500000000000006661 ) ;
#3592 = CARTESIAN_POINT ( 'NONE',  ( 41.14099152588522657, 40.39281886181299797, 84.30501292736984453 ) ) ;
#3593 = CARTESIAN_POINT ( 'NONE',  ( 45.81606138205707879, -39.99575152356564445, 63.13209164280871022 ) ) ;
#3594 = DIRECTION ( 'NONE',  ( 0.000000000000000000, -1.000000000000000000, 2.999999999999999839E-15 ) ) ;
#3595 = ADVANCED_FACE ( 'NONE', ( #4624 ), #14046, .T. ) ;
#3596 = CARTESIAN_POINT ( 'NONE',  ( 44.81606138205700063, -33.05876147765410167, 70.30501292737000085 ) ) ;
#3597 = CARTESIAN_POINT ( 'NONE',  ( 37.38336156205273397, -13.90384086642191264, 70.63227792289247020 ) ) ;
#3598 = CARTESIAN_POINT ( 'NONE',  ( 38.26194895904383486, -1.013682088886101784, 69.64448340153879258 ) ) ;
#3599 = ORIENTED_EDGE ( 'NONE', *, *, #21665, .T. ) ;
#3600 = LINE ( 'NONE', #17021, #21788 ) ;
#3601 = DIRECTION ( 'NONE',  ( 1.000000000000000000, 0.000000000000000000, 0.000000000000000000 ) ) ;
#3602 = ORIENTED_EDGE ( 'NONE', *, *, #20581, .F. ) ;
#3603 = VECTOR ( 'NONE', #20223, 1000.000000000000000 ) ;
#3604 = ORIENTED_EDGE ( 'NONE', *, *, #12267, .F. ) ;
#3605 = CARTESIAN_POINT ( 'NONE',  ( 36.29569395875881099, -28.30384086642192187, 72.77780686321126780 ) ) ;
#3606 = VECTOR ( 'NONE', #12428, 1000.000000000000114 ) ;
#3607 = CARTESIAN_POINT ( 'NONE',  ( 39.37952058850012804, -28.61368208888610454, 70.97781676520600058 ) ) ;
#3608 = CARTESIAN_POINT ( 'NONE',  ( 38.37017380507020192, -6.013682088886110222, 73.71602215082116061 ) ) ;
#3609 = ORIENTED_EDGE ( 'NONE', *, *, #8349, .F. ) ;
#3610 = PLANE ( 'NONE',  #14417 ) ;
#3611 = CARTESIAN_POINT ( 'NONE',  ( 39.24876120206129571, -2.903840866421911304, 72.12822762946750288 ) ) ;
#3612 = SURFACE_STYLE_USAGE ( .BOTH. , #25107 ) ;
#3613 = ORIENTED_EDGE ( 'NONE', *, *, #22495, .T. ) ;
#3614 = DIRECTION ( 'NONE',  ( 0.000000000000000000, 1.000000000000000000, 0.000000000000000000 ) ) ;
#3615 = CARTESIAN_POINT ( 'NONE',  ( 43.31606138205700063, -13.58280000135112964, 20.54174511886706256 ) ) ;
#3616 = CARTESIAN_POINT ( 'NONE',  ( 36.11133435605973574, -10.00384086642191761, 70.60699637195612866 ) ) ;
#3617 = CARTESIAN_POINT ( 'NONE',  ( 47.84183937708599643, -34.55876147765400219, 70.30501292737000085 ) ) ;
#3618 = DIRECTION ( 'NONE',  ( -1.000000000000000000, -1.000000000000000078E-15, 0.000000000000000000 ) ) ;
#3619 = CARTESIAN_POINT ( 'NONE',  ( 36.49096545463212493, -15.51368208888610667, 71.43714994484034264 ) ) ;
#3620 = CARTESIAN_POINT ( 'NONE',  ( 33.63430211860953278, 2.841683824787687218, 6.101742829876973140 ) ) ;
#3621 = CARTESIAN_POINT ( 'NONE',  ( 35.81606138205700063, -29.37462871496113337, 53.20604314849776983 ) ) ;
#3622 = ORIENTED_EDGE ( 'NONE', *, *, #14918, .T. ) ;
#3623 = VECTOR ( 'NONE', #1720, 1000.000000000000000 ) ;
#3624 = FACE_OUTER_BOUND ( 'NONE', #19296, .T. ) ;
#3625 = PRODUCT_RELATED_PRODUCT_CATEGORY ( 'part', '', ( #9935 ) ) ;
#3626 = CARTESIAN_POINT ( 'NONE',  ( 36.80608444377002542, -8.303840866421916544, 72.40698646996135324 ) ) ;
#3627 = SHAPE_DEFINITION_REPRESENTATION ( #13836, #18165 ) ;
#3628 = CARTESIAN_POINT ( 'NONE',  ( 32.99554091088187135, 3.410282305729716246, 6.167518378462418127 ) ) ;
#3629 = CARTESIAN_POINT ( 'NONE',  ( 37.80618814713140097, -19.91368208888610170, 73.13360434286903455 ) ) ;
#3630 = CARTESIAN_POINT ( 'NONE',  ( 46.81606138205707168, -38.13418765192403015, 68.51141129791366780 ) ) ;
#3631 = CARTESIAN_POINT ( 'NONE',  ( 39.29254315202757653, -20.80384086642191832, 72.81632618279321889 ) ) ;
#3632 = CARTESIAN_POINT ( 'NONE',  ( 37.09309150775561648, -5.616297516291425929, 83.29717550927296088 ) ) ;
#3633 = CARTESIAN_POINT ( 'NONE',  ( 39.98359781491296161, -18.41368208888610880, 71.86517103874047052 ) ) ;
#3634 = VERTEX_POINT ( 'NONE', #11328 ) ;
#3635 = CARTESIAN_POINT ( 'NONE',  ( 40.52078840805428683, -24.61368208888610809, 70.60699637195608602 ) ) ;
#3636 = EDGE_LOOP ( 'NONE', ( #1444, #2774, #9496, #19580 ) ) ;
#3637 = DIRECTION ( 'NONE',  ( 0.000000000000000000, -0.5706330172266913525, 0.8212051873014213355 ) ) ;
#3638 = DIRECTION ( 'NONE',  ( -1.000000000000000000, 5.510910596163088391E-31, 1.836970198721029688E-16 ) ) ;
#3639 = AXIS2_PLACEMENT_3D ( 'NONE', #5279, #9032, #24576 ) ;
#3640 = CARTESIAN_POINT ( 'NONE',  ( 38.37017380507018771, -23.60384086642191903, 70.24448340153875847 ) ) ;
#3641 = AXIS2_PLACEMENT_3D ( 'NONE', #13847, #4440, #7932 ) ;
#3642 = ORIENTED_EDGE ( 'NONE', *, *, #3284, .F. ) ;
#3643 = ORIENTED_EDGE ( 'NONE', *, *, #24491, .F. ) ;
#3644 = LINE ( 'NONE', #21431, #13349 ) ;
#3645 = LINE ( 'NONE', #19752, #9608 ) ;
#3646 = DIRECTION ( 'NONE',  ( -1.000000000000000000, -1.000000000000000078E-15, 0.000000000000000000 ) ) ;
#3647 = CARTESIAN_POINT ( 'NONE',  ( 37.25202387243754032, -0.4038408664219159117, 72.75271321436733274 ) ) ;
#3648 = AXIS2_PLACEMENT_3D ( 'NONE', #15451, #11350, #17262 ) ;
#3649 = PLANE ( 'NONE',  #1415 ) ;
#3650 = DIRECTION ( 'NONE',  ( 2.727049986597864201E-15, -0.7516416929448760387, -0.6595716529892418079 ) ) ;
#3651 = ORIENTED_EDGE ( 'NONE', *, *, #15292, .T. ) ;
#3652 = EDGE_CURVE ( 'NONE', #3483, #64, #12743, .T. ) ;
#3653 = AXIS2_PLACEMENT_3D ( 'NONE', #3699, #25328, #23149 ) ;
#3654 = EDGE_LOOP ( 'NONE', ( #4673, #23728, #13093, #24778 ) ) ;
#3655 = EDGE_CURVE ( 'NONE', #2353, #17597, #11195, .T. ) ;
#3656 = CARTESIAN_POINT ( 'NONE',  ( 38.41621794735363693, -36.60729675983900222, 83.30501292737011454 ) ) ;
#3657 = DIRECTION ( 'NONE',  ( 0.000000000000000000, 0.6568589528324747517, -0.7540134720837717852 ) ) ;
#3658 = CARTESIAN_POINT ( 'NONE',  ( 37.69796330110505522, -28.50384086642191761, 73.09843995877328382 ) ) ;
#3659 = SURFACE_STYLE_USAGE ( .BOTH. , #23242 ) ;
#3661 = AXIS2_PLACEMENT_3D ( 'NONE', #24456, #19067, #6828 ) ;
#3660 = DIRECTION ( 'NONE',  ( -1.000000000000000000, 5.510910596163088391E-31, 1.836970198721029688E-16 ) ) ;
#3662 = VECTOR ( 'NONE', #11484, 1000.000000000000000 ) ;
#3663 = ORIENTED_EDGE ( 'NONE', *, *, #11953, .T. ) ;
#3664 = FACE_OUTER_BOUND ( 'NONE', #19556, .T. ) ;
#3665 = DIRECTION ( 'NONE',  ( -2.574571254471601357E-15, 0.8967398287344627850, 0.4425581086832399147 ) ) ;
#3666 = DIRECTION ( 'NONE',  ( -1.000000000000000000, -2.999999999999999839E-15, 0.000000000000000000 ) ) ;
#3667 = CARTESIAN_POINT ( 'NONE',  ( 38.93987200065210175, -4.803840866421909439, 72.33091598616827866 ) ) ;
#3668 = AXIS2_PLACEMENT_3D ( 'NONE', #21864, #12088, #1884 ) ;
#3669 = ORIENTED_EDGE ( 'NONE', *, *, #11478, .F. ) ;
#3670 = EDGE_CURVE ( 'NONE', #5342, #13145, #17251, .T. ) ;
#3671 = CYLINDRICAL_SURFACE ( 'NONE', #852, 0.9999999999999937828 ) ;
#3672 = EDGE_LOOP ( 'NONE', ( #20762, #21747, #5918, #8628 ) ) ;
#3673 = ORIENTED_EDGE ( 'NONE', *, *, #66, .F. ) ;
#3674 = DIRECTION ( 'NONE',  ( 3.717264591378870232E-16, 3.115648231731786715E-15, 1.000000000000000000 ) ) ;
#3675 = VECTOR ( 'NONE', #21739, 1000.000000000000000 ) ;
#3676 = CARTESIAN_POINT ( 'NONE',  ( 38.63098279924288647, -14.91368208888609992, 70.22690120949090442 ) ) ;
#3677 = CIRCLE ( 'NONE', #370, 0.7500000000000014433 ) ;
#3678 = CARTESIAN_POINT ( 'NONE',  ( 39.37952058850012804, -12.61368208888609921, 70.97781676520601479 ) ) ;
#3679 = EDGE_LOOP ( 'NONE', ( #21342, #2303, #5473, #14109 ) ) ;
#3680 = ORIENTED_EDGE ( 'NONE', *, *, #9929, .F. ) ;
#3681 = CARTESIAN_POINT ( 'NONE',  ( 36.56606138205700063, 5.308699250829721272, 2.416607620847027960 ) ) ;
#3682 = CARTESIAN_POINT ( 'NONE',  ( 32.84131651066541480, -32.95845724189726411, 59.23979596822106686 ) ) ;
#3683 = VERTEX_POINT ( 'NONE', #15041 ) ;
#3684 = CARTESIAN_POINT ( 'NONE',  ( 44.81606138205700063, 41.44123852234599781, 75.30501292736987295 ) ) ;
#3685 = CARTESIAN_POINT ( 'NONE',  ( 39.38009889167648936, -17.40384086642190908, 70.00779233799262613 ) ) ;
#3686 = CIRCLE ( 'NONE', #21376, 1.249999999999995115 ) ;
#3687 = DIRECTION ( 'NONE',  ( 1.000000000000000000, 3.965082230804126670E-15, 0.000000000000000000 ) ) ;
#3688 = CARTESIAN_POINT ( 'NONE',  ( 37.12184278917507640, -21.51368208888609956, 71.43714994484034264 ) ) ;
#3689 = CIRCLE ( 'NONE', #13154, 0.7500000000000006661 ) ;
#3690 = ORIENTED_EDGE ( 'NONE', *, *, #17616, .T. ) ;
#3691 = ORIENTED_EDGE ( 'NONE', *, *, #12095, .F. ) ;
#3692 = CARTESIAN_POINT ( 'NONE',  ( 36.81465384343994884, 40.76768529863396395, 79.37823623207322044 ) ) ;
#3693 = CARTESIAN_POINT ( 'NONE',  ( 31.81606138205700418, 0.1601050959395486362, 68.80395113470939350 ) ) ;
#3694 = FACE_OUTER_BOUND ( 'NONE', #8093, .T. ) ;
#3695 = AXIS2_PLACEMENT_3D ( 'NONE', #8825, #18351, #4943 ) ;
#3696 = CARTESIAN_POINT ( 'NONE',  ( 39.82611197195675601, -5.886287209492222949, 83.28324666752695293 ) ) ;
#3697 = CARTESIAN_POINT ( 'NONE',  ( 33.31606138205700773, -40.62725863591898445, 68.52362519861142687 ) ) ;
#3698 = AXIS2_PLACEMENT_3D ( 'NONE', #2196, #17674, #4011 ) ;
#3699 = CARTESIAN_POINT ( 'NONE',  ( 43.81606138205700063, -20.88462213363798270, 44.49284693533410717 ) ) ;
#3700 = ADVANCED_FACE ( 'NONE', ( #24818, #19044 ), #25062, .F. ) ;
#3701 = CARTESIAN_POINT ( 'NONE',  ( 30.81606138205706458, -34.54722833698622964, 70.28164373264664277 ) ) ;
#3702 = EDGE_LOOP ( 'NONE', ( #3708, #18334, #10522, #3953 ) ) ;
#3703 = ORIENTED_EDGE ( 'NONE', *, *, #9232, .T. ) ;
#3704 = CARTESIAN_POINT ( 'NONE',  ( 35.86008812008917346, -8.103840866421913702, 71.32335560751961623 ) ) ;
#3705 = CARTESIAN_POINT ( 'NONE',  ( 45.81606138205695800, -0.2703287878657676391, 1.505452687840413972 ) ) ;
#3706 = CARTESIAN_POINT ( 'NONE',  ( 36.49096545463212493, -13.51368208888610489, 71.43714994484034264 ) ) ;
#3707 = CIRCLE ( 'NONE', #22642, 0.7500000000000014433 ) ;
#3708 = ORIENTED_EDGE ( 'NONE', *, *, #11770, .F. ) ;
#3709 = CARTESIAN_POINT ( 'NONE',  ( 29.81606138205706458, -34.55876147768187678, 70.30501292735635843 ) ) ;
#3710 = CARTESIAN_POINT ( 'NONE',  ( 35.14099152588523367, -10.60718113818700026, 93.30501292736998664 ) ) ;
#3711 = CARTESIAN_POINT ( 'NONE',  ( 35.86008812008917346, -23.51368208888609956, 71.43714994484032843 ) ) ;
#3712 = VERTEX_POINT ( 'NONE', #16185 ) ;
#3713 = ADVANCED_FACE ( 'NONE', ( #8212 ), #15810, .F. ) ;
#3714 = FACE_BOUND ( 'NONE', #15584, .T. ) ;
#3715 = CARTESIAN_POINT ( 'NONE',  ( 45.81606138205697221, -4.589472609077215992, -6.350807634294793225 ) ) ;
#3716 = CARTESIAN_POINT ( 'NONE',  ( 43.31606138205700063, 7.864187680719676443, 65.89022736311019912 ) ) ;
#3717 = EDGE_CURVE ( 'NONE', #5857, #7071, #209, .T. ) ;
#3718 = EDGE_CURVE ( 'NONE', #14544, #24541, #22999, .T. ) ;
#3719 = EDGE_CURVE ( 'NONE', #17105, #16154, #6279, .T. ) ;
#3720 = ADVANCED_FACE ( 'NONE', ( #17750 ), #21737, .T. ) ;
#3721 = FILL_AREA_STYLE ('',( #6179 ) ) ;
#3722 = VECTOR ( 'NONE', #21598, 1000.000000000000000 ) ;
#3723 = PLANE ( 'NONE',  #5296 ) ;
#3724 = DIRECTION ( 'NONE',  ( 0.000000000000000000, 0.000000000000000000, 1.000000000000000000 ) ) ;
#3725 = VECTOR ( 'NONE', #17094, 1000.000000000000000 ) ;
#3726 = CARTESIAN_POINT ( 'NONE',  ( 39.24876120206129571, -12.90384086642191264, 72.12822762946747446 ) ) ;
#3727 = CARTESIAN_POINT ( 'NONE',  ( 37.38336156205274818, -27.71368208888610241, 72.12822762946747446 ) ) ;
#3728 = EDGE_LOOP ( 'NONE', ( #3768, #15281, #4821, #15902 ) ) ;
#3729 = CYLINDRICAL_SURFACE ( 'NONE', #20555, 2.500000000000002220 ) ;
#3730 = EDGE_CURVE ( 'NONE', #24147, #18393, #12212, .T. ) ;
#3731 = CARTESIAN_POINT ( 'NONE',  ( 41.81606138205696510, -1.975699482566714904, -4.057200616784870206 ) ) ;
#3732 = VERTEX_POINT ( 'NONE', #14139 ) ;
#3733 = ORIENTED_EDGE ( 'NONE', *, *, #1251, .T. ) ;
#3734 = CARTESIAN_POINT ( 'NONE',  ( 39.95015449827720744, 0.9961591335780894951, 71.96809898377890136 ) ) ;
#3735 = CARTESIAN_POINT ( 'NONE',  ( 39.29254315202756231, -0.8136820888860994971, 69.94417936956673998 ) ) ;
#3736 = B_SPLINE_SURFACE_WITH_KNOTS ( 'NONE', 1, 3, ( 
 ( #5509, #5756, #19158, #11700, #1617, #3310, #5628 ),
 ( #7310, #13374, #25179, #15161, #11186, #13489, #21221 ),
 ( #1495, #7823, #17231, #15669, #19539, #19034, #3557 ) ),
 .UNSPECIFIED., .F., .F., .F.,
 ( 2, 1, 2 ),
 ( 4, 3, 4 ),
 ( -0.01000000000000000021, 0.000000000000000000, 1.000000000000000000 ),
 ( 0.000000000000000000, 1.000000000000000000, 1.010000000000000009 ),
 .UNSPECIFIED. ) ;
#3737 = CARTESIAN_POINT ( 'NONE',  ( 40.33642880535524000, -0.3136820888861093781, 72.77780686321128201 ) ) ;
#3738 = EDGE_LOOP ( 'NONE', ( #5619, #20576 ) ) ;
#3739 = CARTESIAN_POINT ( 'NONE',  ( 43.81606138205700063, 2.191238522346988127, 65.30501292737000085 ) ) ;
#3740 = CARTESIAN_POINT ( 'NONE',  ( 37.31647492878124694, -4.303840866421912992, 72.03616607671141026 ) ) ;
#3741 = CARTESIAN_POINT ( 'NONE',  ( 43.81606138205700063, 6.699978067258562042, 7.424159817622362212 ) ) ;
#3742 = EDGE_LOOP ( 'NONE', ( #3280, #18043, #11656, #21146 ) ) ;
#3743 = CYLINDRICAL_SURFACE ( 'NONE', #22838, 1.000000000000000000 ) ;
#3744 = DIRECTION ( 'NONE',  ( 0.000000000000000000, -0.3299742535180970049, 0.9439899321577400748 ) ) ;
#3745 = CARTESIAN_POINT ( 'NONE',  ( 39.64521430340305841, -10.80384086642191832, 73.30173637941818754 ) ) ;
#3746 = VECTOR ( 'NONE', #17871, 1000.000000000000000 ) ;
#3747 = PLANE ( 'NONE',  #8647 ) ;
#3748 = FILL_AREA_STYLE_COLOUR ( '', #14877 ) ;
#3749 = CARTESIAN_POINT ( 'NONE',  ( 36.87297107704152666, -11.71368208888611129, 72.49904802271740323 ) ) ;
#3750 = DIRECTION ( 'NONE',  ( 0.000000000000000000, -0.5706330172266919076, 0.8212051873014208914 ) ) ;
#3751 = CARTESIAN_POINT ( 'NONE',  ( 35.64099152588522657, 1.392818861812999964, 83.30501292736997243 ) ) ;
#3752 = EDGE_CURVE ( 'NONE', #5864, #17161, #2432, .T. ) ;
#3753 = ORIENTED_EDGE ( 'NONE', *, *, #23120, .F. ) ;
#3754 = ADVANCED_FACE ( 'NONE', ( #25456, #7834, #17885 ), #5898, .T. ) ;
#3755 = DIRECTION ( 'NONE',  ( 1.734723475976804876E-16, 3.491481338843135327E-15, 1.000000000000000000 ) ) ;
#3756 = CARTESIAN_POINT ( 'NONE',  ( 37.69796330110505522, -4.503840866421914946, 73.09843995877331224 ) ) ;
#3757 = PRODUCT_CONTEXT ( 'NONE', #22302, 'mechanical' ) ;
#3758 = DIRECTION ( 'NONE',  ( 0.000000000000000000, -0.8212051873014208914, -0.5706330172266919076 ) ) ;
#3759 = CARTESIAN_POINT ( 'NONE',  ( 39.29254315202756231, -16.81368208888610383, 69.94417936956672577 ) ) ;
#3760 = DIRECTION ( 'NONE',  ( 1.000000000000000000, 0.000000000000000000, 0.000000000000000000 ) ) ;
#3761 = ADVANCED_FACE ( 'NONE', ( #14262 ), #15928, .F. ) ;
#3762 = CARTESIAN_POINT ( 'NONE',  ( 36.49096545463212493, -18.10384086642191193, 71.32335560751961623 ) ) ;
#3763 = CARTESIAN_POINT ( 'NONE',  ( 38.18531088334250967, -5.204193249396277032, 83.30501292736992980 ) ) ;
#3764 = VECTOR ( 'NONE', #17293, 1000.000000000000000 ) ;
#3765 = CARTESIAN_POINT ( 'NONE',  ( 38.26194895904383486, -17.01368208888610312, 69.64448340153877837 ) ) ;
#3766 = VERTEX_POINT ( 'NONE', #23785 ) ;
#3767 = CARTESIAN_POINT ( 'NONE',  ( 39.12911128074873801, -22.11368208888610809, 73.69843995877327814 ) ) ;
#3768 = ORIENTED_EDGE ( 'NONE', *, *, #18547, .F. ) ;
#3769 = LINE ( 'NONE', #21179, #9893 ) ;
#3770 = DIRECTION ( 'NONE',  ( 7.071067811865460542E-16, -0.4341746501209495790, -0.9008287146801832179 ) ) ;
#3771 = CARTESIAN_POINT ( 'NONE',  ( 39.31564783533279694, -27.30384086642191477, 70.72433947564850598 ) ) ;
#3772 = ORIENTED_EDGE ( 'NONE', *, *, #6897, .T. ) ;
#3773 = EDGE_CURVE ( 'NONE', #194, #22820, #24037, .T. ) ;
#3774 = EDGE_LOOP ( 'NONE', ( #21500, #4957, #18878, #15099, #18536, #11335, #278, #18169, #9610, #186, #20133, #5812 ) ) ;
#3775 = CARTESIAN_POINT ( 'NONE',  ( 31.81606138205700418, -27.70293563151089700, 74.66612024218476051 ) ) ;
#3776 = CARTESIAN_POINT ( 'NONE',  ( 44.06606138205700063, -26.74044063519535186, 83.30501292737007191 ) ) ;
#3777 = FILL_AREA_STYLE_COLOUR ( '', #11896 ) ;
#3778 = CARTESIAN_POINT ( 'NONE',  ( 35.86008812008917346, -28.10384086642191903, 71.32335560751960202 ) ) ;
#3779 = CARTESIAN_POINT ( 'NONE',  ( 36.31606138205700063, -22.22127907754180853, 85.30501292736998664 ) ) ;
#3780 = CARTESIAN_POINT ( 'NONE',  ( 36.29569395875879678, -5.313682088886097610, 69.98269868914869107 ) ) ;
#3781 = AXIS2_PLACEMENT_3D ( 'NONE', #12203, #6014, #18125 ) ;
#3782 = FACE_OUTER_BOUND ( 'NONE', #23471, .T. ) ;
#3783 = AXIS2_PLACEMENT_3D ( 'NONE', #9531, #17375, #1894 ) ;
#3784 = ORIENTED_EDGE ( 'NONE', *, *, #3255, .T. ) ;
#3785 = VERTEX_POINT ( 'NONE', #10145 ) ;
#3786 = CARTESIAN_POINT ( 'NONE',  ( 33.80700705136447937, 3.227014435054107455, 6.369498925975481285 ) ) ;
#3787 = CARTESIAN_POINT ( 'NONE',  ( 31.81606138205700418, 41.44123852234595518, 61.30501292736988006 ) ) ;
#3788 = CIRCLE ( 'NONE', #10792, 3.000000000000000000 ) ;
#3789 = CARTESIAN_POINT ( 'NONE',  ( 38.82593461698264292, -22.70384086642191690, 73.13360434286903455 ) ) ;
#3790 = FACE_OUTER_BOUND ( 'NONE', #12242, .T. ) ;
#3791 = VERTEX_POINT ( 'NONE', #6153 ) ;
#3792 = CARTESIAN_POINT ( 'NONE',  ( 38.31606138205700063, 0.6124887759231013584, 81.37823623207334833 ) ) ;
#3793 = CARTESIAN_POINT ( 'NONE',  ( 33.31606138205700773, 7.187001342539796944, 66.09667597968754649 ) ) ;
#3794 = CARTESIAN_POINT ( 'NONE',  ( 43.81608638205700146, -3.566646240838321269, 18.16837712155798457 ) ) ;
#3795 = CARTESIAN_POINT ( 'NONE',  ( 38.00113996487112189, -3.703840866421909794, 70.22690120949091863 ) ) ;
#3796 = ORIENTED_EDGE ( 'NONE', *, *, #23732, .T. ) ;
#3797 = CARTESIAN_POINT ( 'NONE',  ( 41.31606138205700063, 3.392460599465057403, 64.84545171350526971 ) ) ;
#3798 = ORIENTED_EDGE ( 'NONE', *, *, #24971, .F. ) ;
#3799 = ORIENTED_EDGE ( 'NONE', *, *, #6026, .T. ) ;
#3800 = CIRCLE ( 'NONE', #16984, 1.000000000000000888 ) ;
#3802 = ADVANCED_FACE ( 'NONE', ( #21613 ), #14012, .T. ) ;
#3801 = CARTESIAN_POINT ( 'NONE',  ( 41.31606138205700063, 7.283211578144648257, 66.04722806671131252 ) ) ;
#3803 = CARTESIAN_POINT ( 'NONE',  ( 37.21915885897815457, -9.413682088886103472, 71.08074471024443142 ) ) ;
#3804 = EDGE_CURVE ( 'NONE', #12702, #24067, #331, .T. ) ;
#3805 = CARTESIAN_POINT ( 'NONE',  ( 37.31647492878122563, -11.31368208888609850, 70.72433947564853440 ) ) ;
#3806 = ORIENTED_EDGE ( 'NONE', *, *, #2623, .T. ) ;
#3807 = ADVANCED_FACE ( 'NONE', ( #17626 ), #10461, .T. ) ;
#3808 = VERTEX_POINT ( 'NONE', #11471 ) ;
#3809 = CARTESIAN_POINT ( 'NONE',  ( 44.81606138205700063, -34.55876147765410167, 70.30501292737000085 ) ) ;
#3810 = VECTOR ( 'NONE', #24922, 1000.000000000000000 ) ;
#3811 = PLANE ( 'NONE',  #7511 ) ;
#3812 = ORIENTED_EDGE ( 'NONE', *, *, #19506, .F. ) ;
#3813 = DIRECTION ( 'NONE',  ( -1.000000000000000000, -2.999999999999999839E-15, 0.000000000000000000 ) ) ;
#3814 = CARTESIAN_POINT ( 'NONE',  ( 37.25202387243754032, -18.40384086642191974, 72.75271321436731853 ) ) ;
#3815 = DIRECTION ( 'NONE',  ( -1.734723475976804876E-16, -3.491481338843135327E-15, -1.000000000000000000 ) ) ;
#3816 = AXIS2_PLACEMENT_3D ( 'NONE', #24713, #13019, #20872 ) ;
#3817 = VECTOR ( 'NONE', #19823, 1000.000000000000000 ) ;
#3818 = CARTESIAN_POINT ( 'NONE',  ( 37.31647492878122563, -17.31368208888610383, 70.72433947564853440 ) ) ;
#3819 = ORIENTED_EDGE ( 'NONE', *, *, #16170, .T. ) ;
#3820 = ORIENTED_EDGE ( 'NONE', *, *, #10423, .F. ) ;
#3821 = VERTEX_POINT ( 'NONE', #13648 ) ;
#3822 = DIRECTION ( 'NONE',  ( -1.000000000000000000, -1.734723475976804876E-16, 1.734723475976814737E-16 ) ) ;
#3823 = CARTESIAN_POINT ( 'NONE',  ( 38.82593461698262871, -10.91368208888610170, 69.62690120949091011 ) ) ;
#3824 = ADVANCED_FACE ( 'NONE', ( #11597 ), #15319, .T. ) ;
#3825 = AXIS2_PLACEMENT_3D ( 'NONE', #19613, #1956, #21181 ) ;
#3826 = CYLINDRICAL_SURFACE ( 'NONE', #5656, 0.7500000000000006661 ) ;
#3827 = CARTESIAN_POINT ( 'NONE',  ( 43.79080625344859357, -32.95845724189726411, 59.23979596822106686 ) ) ;
#3828 = CARTESIAN_POINT ( 'NONE',  ( 43.81606138205700063, -24.55876147765401285, 70.30501292737008612 ) ) ;
#3829 = DIRECTION ( 'NONE',  ( 0.000000000000000000, 2.999999999999999839E-15, 1.000000000000000000 ) ) ;
#3830 = AXIS2_PLACEMENT_3D ( 'NONE', #14969, #5311, #14584 ) ;
#3831 = DIRECTION ( 'NONE',  ( 1.000000000000000000, 8.911169920151748851E-16, 3.114923731923493702E-16 ) ) ;
#3832 = ORIENTED_EDGE ( 'NONE', *, *, #22638, .T. ) ;
#3833 = VECTOR ( 'NONE', #19930, 1000.000000000000000 ) ;
#3834 = CARTESIAN_POINT ( 'NONE',  ( 35.14099152588522657, -10.60718113818700026, 83.30501292737001506 ) ) ;
#3835 = VERTEX_POINT ( 'NONE', #5541 ) ;
#3836 = EDGE_LOOP ( 'NONE', ( #2495, #14993, #21778, #3968 ) ) ;
#3837 = CARTESIAN_POINT ( 'NONE',  ( 39.12911128074872380, -13.50384086642191228, 69.06206559358665231 ) ) ;
#3838 =( GEOMETRIC_REPRESENTATION_CONTEXT ( 3 ) GLOBAL_UNCERTAINTY_ASSIGNED_CONTEXT ( ( #12881 ) ) GLOBAL_UNIT_ASSIGNED_CONTEXT ( ( #19182, #25209, #13515 ) ) REPRESENTATION_CONTEXT ( 'NONE', 'WORKASPACE' ) );
#3839 = VERTEX_POINT ( 'NONE', #13401 ) ;
#3840 = CARTESIAN_POINT ( 'NONE',  ( 32.56606138205700773, 43.04446929126255128, 81.37823623207322044 ) ) ;
#3841 = CARTESIAN_POINT ( 'NONE',  ( 39.29254315202756231, -16.81368208888610383, 69.94417936956672577 ) ) ;
#3842 = AXIS2_PLACEMENT_3D ( 'NONE', #19111, #7256, #23464 ) ;
#3843 = SHAPE_REPRESENTATION_RELATIONSHIP ( 'NONE' , 'NONE' ,  #4169, #10468 ) ;
#3844 = ORIENTED_EDGE ( 'NONE', *, *, #9003, .F. ) ;
#3845 = DIRECTION ( 'NONE',  ( 1.000000000000000000, 0.000000000000000000, 0.000000000000000000 ) ) ;
#3846 = CARTESIAN_POINT ( 'NONE',  ( 41.31606138205700063, 8.104266321858618838, 55.82104096753806033 ) ) ;
#3847 = CIRCLE ( 'NONE', #13730, 0.7499999999999983347 ) ;
#3848 = CARTESIAN_POINT ( 'NONE',  ( 40.77203464402485622, -24.51368208888610667, 71.32335560751960202 ) ) ;
#3849 = EDGE_LOOP ( 'NONE', ( #1772, #15717, #7269, #22855 ) ) ;
#3850 = CARTESIAN_POINT ( 'NONE',  ( 33.31606138205700773, -20.88462213365835041, 44.49284693532412405 ) ) ;
#3851 = CARTESIAN_POINT ( 'NONE',  ( 46.81606138205697221, -3.984974717493081187, -3.847356352999882656 ) ) ;
#3852 = LINE ( 'NONE', #13276, #21098 ) ;
#3853 = CIRCLE ( 'NONE', #12913, 3.000000000000000000 ) ;
#3854 = EDGE_CURVE ( 'NONE', #8842, #21203, #13959, .T. ) ;
#3855 = ORIENTED_EDGE ( 'NONE', *, *, #20566, .F. ) ;
#3856 = DIRECTION ( 'NONE',  ( 0.000000000000000000, 1.000000000000000000, 0.000000000000000000 ) ) ;
#3857 = PRESENTATION_LAYER_ASSIGNMENT (  '', '', ( #25242 ) ) ;
#3858 = DIRECTION ( 'NONE',  ( -0.1733269559585509378, 0.000000000000000000, -0.9848643390529188135 ) ) ;
#3859 = AXIS2_PLACEMENT_3D ( 'NONE', #2045, #3860, #19573 ) ;
#3860 = DIRECTION ( 'NONE',  ( 1.000000000000000000, 1.734723475976799945E-16, -1.734723475976814737E-16 ) ) ;
#3861 = CARTESIAN_POINT ( 'NONE',  ( 38.93987200065210175, -14.80384086642191122, 72.33091598616826445 ) ) ;
#3862 = CARTESIAN_POINT ( 'NONE',  ( 38.37017380507020192, -0.01368208888610777940, 73.11602215082118050 ) ) ;
#3863 = VERTEX_POINT ( 'NONE', #23045 ) ;
#3864 = DIRECTION ( 'NONE',  ( 1.927470528863119788E-16, 1.000000000000000000, -2.999999999999999839E-15 ) ) ;
#3865 = CIRCLE ( 'NONE', #7581, 1.000000000000011990 ) ;
#3866 = DIRECTION ( 'NONE',  ( 1.000000000000000000, 2.452751524064190075E-15, 1.339444584486322859E-15 ) ) ;
#3867 = ORIENTED_EDGE ( 'NONE', *, *, #11453, .F. ) ;
#3868 = ORIENTED_EDGE ( 'NONE', *, *, #12339, .F. ) ;
#3869 = CARTESIAN_POINT ( 'NONE',  ( 37.50301148336529877, -28.50384086642192116, 73.69843995877326392 ) ) ;
#3870 = CARTESIAN_POINT ( 'NONE',  ( 37.89291511884476904, -23.11368208888610454, 70.26206559358661252 ) ) ;
#3871 = CARTESIAN_POINT ( 'NONE',  ( 38.26194895904383486, -5.013682088886101340, 69.04448340153881247 ) ) ;
#3872 = VERTEX_POINT ( 'NONE', #5410 ) ;
#3873 = DIRECTION ( 'NONE',  ( -1.000000000000000000, 5.510910596163088391E-31, 1.836970198721029688E-16 ) ) ;
#3874 = CARTESIAN_POINT ( 'NONE',  ( 39.02742774030101458, -3.403840866421911748, 70.49320253461759478 ) ) ;
#3875 = EDGE_CURVE ( 'NONE', #21859, #2986, #23169, .T. ) ;
#3876 = APPLICATION_CONTEXT ( 'automotive_design' ) ;
#3877 = CARTESIAN_POINT ( 'NONE',  ( 39.02088643472237095, -2.913682088886100363, 69.02690120949094421 ) ) ;
#3878 = CARTESIAN_POINT ( 'NONE',  ( 43.81606138205700063, -37.34243788671330577, 70.80615726751818784 ) ) ;
#3879 = VERTEX_POINT ( 'NONE', #21248 ) ;
#3880 = DIRECTION ( 'NONE',  ( 1.445602896647339656E-16, -0.8212051873014208914, -0.5706330172266919076 ) ) ;
#3881 = CARTESIAN_POINT ( 'NONE',  ( 45.81606138205700063, 40.39281886181299797, 82.55501292736983032 ) ) ;
#3882 = CARTESIAN_POINT ( 'NONE',  ( 39.12911128074872380, -9.503840866421912281, 69.06206559358666652 ) ) ;
#3883 = CIRCLE ( 'NONE', #18291, 1.000000000000000888 ) ;
#3884 = LINE ( 'NONE', #19594, #15639 ) ;
#3885 = DIRECTION ( 'NONE',  ( 0.000000000000000000, -0.5735764363510463815, 0.8191520442889914655 ) ) ;
#3886 = CARTESIAN_POINT ( 'NONE',  ( 37.25202387243752611, -15.21368208888610063, 70.00779233799262613 ) ) ;
#3887 = CARTESIAN_POINT ( 'NONE',  ( 44.81606138205700063, -34.55876147765400219, 74.30501292737011454 ) ) ;
#3888 = AXIS2_PLACEMENT_3D ( 'NONE', #5596, #23232, #15884 ) ;
#3889 = EDGE_CURVE ( 'NONE', #4384, #17348, #7469, .T. ) ;
#3890 = DIRECTION ( 'NONE',  ( 0.000000000000000000, 0.000000000000000000, 1.000000000000000000 ) ) ;
#3891 = CARTESIAN_POINT ( 'NONE',  ( 32.56606138205700773, 40.39281886181299797, 82.55501292736983032 ) ) ;
#3892 = CARTESIAN_POINT ( 'NONE',  ( 37.80618814713138676, -3.703840866421905798, 69.62690120949091011 ) ) ;
#3893 = ITEM_DEFINED_TRANSFORMATION ( 'NONE', 'NONE', #10069,  #2000 ) ;
#3894 = CARTESIAN_POINT ( 'NONE',  ( 43.19824457581059107, 3.616009060170059630, 6.335949910530210616 ) ) ;
#3895 = CARTESIAN_POINT ( 'NONE',  ( 39.29254315202756231, -20.81368208888610027, 69.94417936956672577 ) ) ;
#3896 = LINE ( 'NONE', #23842, #15599 ) ;
#3897 = AXIS2_PLACEMENT_3D ( 'NONE', #5051, #13173, #20777 ) ;
#3898 = CARTESIAN_POINT ( 'NONE',  ( 37.69796330110505522, -20.50384086642191050, 73.09843995877329803 ) ) ;
#3899 = EDGE_CURVE ( 'NONE', #21678, #1971, #19068, .T. ) ;
#3900 = CARTESIAN_POINT ( 'NONE',  ( 44.81606138205700063, -36.30035594811090505, 74.91924054225879104 ) ) ;
#3901 = ADVANCED_FACE ( 'NONE', ( #1646 ), #9539, .T. ) ;
#3902 = CARTESIAN_POINT ( 'NONE',  ( 38.26194895904383486, -15.01368208888610134, 69.64448340153877837 ) ) ;
#3903 = ORIENTED_EDGE ( 'NONE', *, *, #3889, .T. ) ;
#3904 = CARTESIAN_POINT ( 'NONE',  ( 39.02088643472237095, -20.91368208888609814, 69.02690120949091579 ) ) ;
#3905 = ORIENTED_EDGE ( 'NONE', *, *, #2203, .T. ) ;
#3906 = DIRECTION ( 'NONE',  ( -1.000000000000000000, -1.000000000000000078E-15, 0.000000000000000000 ) ) ;
#3907 = EDGE_CURVE ( 'NONE', #10892, #20855, #23427, .T. ) ;
#3908 = CARTESIAN_POINT ( 'NONE',  ( 45.81606138205697931, -6.382952266546141118, -7.235923851661270945 ) ) ;
#3909 = CARTESIAN_POINT ( 'NONE',  ( 38.73920764526923932, -21.50384086642191406, 70.26206559358661252 ) ) ;
#3910 = EDGE_CURVE ( 'NONE', #2302, #13705, #25036, .T. ) ;
#3911 = ORIENTED_EDGE ( 'NONE', *, *, #4063, .F. ) ;
#3912 = ORIENTED_EDGE ( 'NONE', *, *, #2151, .F. ) ;
#3913 = CARTESIAN_POINT ( 'NONE',  ( 39.59324923284151510, -28.74115096347518161, 70.20355626897213597 ) ) ;
#3914 = CARTESIAN_POINT ( 'NONE',  ( 44.81606138205700063, 31.19260082947834078, 104.9690409559304101 ) ) ;
#3915 = ORIENTED_EDGE ( 'NONE', *, *, #22950, .F. ) ;
#3916 = CARTESIAN_POINT ( 'NONE',  ( 36.80608444377001831, -0.3038408664219130473, 72.40698646996136745 ) ) ;
#3917 = DIRECTION ( 'NONE',  ( 0.2503287245161955887, 0.9681609007195522976, -3.423740829372836395E-15 ) ) ;
#3918 = CARTESIAN_POINT ( 'NONE',  ( 40.33642880535524000, -2.313682088886106936, 72.77780686321128201 ) ) ;
#3919 = EDGE_CURVE ( 'NONE', #9104, #20720, #19566, .T. ) ;
#3920 = FACE_OUTER_BOUND ( 'NONE', #13367, .T. ) ;
#3921 = VECTOR ( 'NONE', #4641, 1000.000000000000000 ) ;
#3922 = ADVANCED_FACE ( 'NONE', ( #21372 ), #23415, .T. ) ;
#3923 = ORIENTED_EDGE ( 'NONE', *, *, #19323, .T. ) ;
#3924 = ORIENTED_EDGE ( 'NONE', *, *, #22580, .F. ) ;
#3925 = FACE_OUTER_BOUND ( 'NONE', #4632, .T. ) ;
#3926 = PLANE ( 'NONE',  #16328 ) ;
#3927 = CARTESIAN_POINT ( 'NONE',  ( 36.49096545463212493, -18.10384086642191193, 71.32335560751961623 ) ) ;
#3928 = PRESENTATION_STYLE_ASSIGNMENT (( #3659 ) ) ;
#3929 = CARTESIAN_POINT ( 'NONE',  ( 42.06606138205700063, 42.19123852234599781, 74.30501292736987295 ) ) ;
#3930 = ORIENTED_EDGE ( 'NONE', *, *, #12883, .T. ) ;
#3931 = DIRECTION ( 'NONE',  ( 1.000000000000000000, 0.000000000000000000, -0.000000000000000000 ) ) ;
#3932 = EDGE_CURVE ( 'NONE', #7931, #1075, #25345, .T. ) ;
#3933 = DIRECTION ( 'NONE',  ( -1.301042606982603842E-16, 0.000000000000000000, -1.000000000000000000 ) ) ;
#3934 = CARTESIAN_POINT ( 'NONE',  ( 45.06606138205697221, -5.022037326221688858, -5.474317061061731771 ) ) ;
#3935 = CARTESIAN_POINT ( 'NONE',  ( 39.37952058850012804, -7.003840866421911393, 71.78268878715392987 ) ) ;
#3936 = VERTEX_POINT ( 'NONE', #5789 ) ;
#3937 = DIRECTION ( 'NONE',  ( 1.000000000000000000, 4.336808689942014655E-17, -1.734723475976809806E-16 ) ) ;
#3938 = VERTEX_POINT ( 'NONE', #9296 ) ;
#3939 = ORIENTED_EDGE ( 'NONE', *, *, #13826, .T. ) ;
#3940 = DIRECTION ( 'NONE',  ( -1.327674326049719602E-15, 0.4425581086832399147, -0.8967398287344627850 ) ) ;
#3941 = CARTESIAN_POINT ( 'NONE',  ( 38.00113996487114321, -11.91368208888610170, 72.53360434286904024 ) ) ;
#3942 = CARTESIAN_POINT ( 'NONE',  ( 38.93987200065208754, -12.81368208888610383, 70.42958956619168021 ) ) ;
#3943 = ORIENTED_EDGE ( 'NONE', *, *, #17763, .F. ) ;
#3944 = ORIENTED_EDGE ( 'NONE', *, *, #16305, .T. ) ;
#3945 = FACE_OUTER_BOUND ( 'NONE', #10813, .T. ) ;
#3946 = FACE_OUTER_BOUND ( 'NONE', #19029, .T. ) ;
#3947 = ORIENTED_EDGE ( 'NONE', *, *, #13341, .T. ) ;
#3948 = CYLINDRICAL_SURFACE ( 'NONE', #22674, 2.000000000000000888 ) ;
#3949 = CARTESIAN_POINT ( 'NONE',  ( 36.68196826583682935, -18.00384086642191406, 70.79240656858107172 ) ) ;
#3950 = CARTESIAN_POINT ( 'NONE',  ( 43.06606138205700063, 41.44123852234599781, 75.30501292736987295 ) ) ;
#3951 = LINE ( 'NONE', #21605, #16212 ) ;
#3952 = CARTESIAN_POINT ( 'NONE',  ( 37.25260217561390874, -17.61368208888609743, 71.78268878715392987 ) ) ;
#3953 = ORIENTED_EDGE ( 'NONE', *, *, #11175, .F. ) ;
#3954 = ORIENTED_EDGE ( 'NONE', *, *, #12871, .F. ) ;
#3955 = CARTESIAN_POINT ( 'NONE',  ( 38.83610899671118943, -5.268488250605326328, 83.30484769703562620 ) ) ;
#3956 = CARTESIAN_POINT ( 'NONE',  ( 36.64852494920107517, -13.41368208888610525, 70.89533451361947414 ) ) ;
#3957 = DIRECTION ( 'NONE',  ( 0.000000000000000000, 1.000000000000000000, 0.000000000000000000 ) ) ;
#3958 = EDGE_CURVE ( 'NONE', #15554, #13947, #17136, .T. ) ;
#3959 = DIRECTION ( 'NONE',  ( 1.000000000000000000, 0.000000000000000000, 0.000000000000000000 ) ) ;
#3960 = EDGE_CURVE ( 'NONE', #19561, #7627, #19191, .T. ) ;
#3961 = VECTOR ( 'NONE', #2199, 1000.000000000000000 ) ;
#3962 = CARTESIAN_POINT ( 'NONE',  ( 39.95015449827720744, -28.61368208888610454, 70.79240656858104330 ) ) ;
#3963 = FACE_OUTER_BOUND ( 'NONE', #11280, .T. ) ;
#3964 = PRODUCT ( 'Anvil Plate', 'Anvil Plate', '', ( #21040 ) ) ;
#3965 = DIRECTION ( 'NONE',  ( -1.734723475976804876E-16, 0.8212051873014210024, 0.5706330172266920187 ) ) ;
#3966 = ORIENTED_EDGE ( 'NONE', *, *, #13822, .F. ) ;
#3967 = CARTESIAN_POINT ( 'NONE',  ( 43.39072112803988546, 3.102161780314388828, 6.136388117020111999 ) ) ;
#3968 = ORIENTED_EDGE ( 'NONE', *, *, #24575, .T. ) ;
#3969 = ORIENTED_EDGE ( 'NONE', *, *, #8801, .F. ) ;
#3970 = CARTESIAN_POINT ( 'NONE',  ( 36.36258059203030513, -3.903840866421911748, 69.89063713639259845 ) ) ;
#3971 = ORIENTED_EDGE ( 'NONE', *, *, #2927, .T. ) ;
#3972 = CARTESIAN_POINT ( 'NONE',  ( 43.31606138205700063, -12.97731741051367393, 21.08248588348817876 ) ) ;
#3973 = CARTESIAN_POINT ( 'NONE',  ( 39.75915168707250302, -16.71368208888609885, 70.26145752964251301 ) ) ;
#3974 = ORIENTED_EDGE ( 'NONE', *, *, #11326, .T. ) ;
#3975 = LINE ( 'NONE', #24950, #10933 ) ;
#3976 = CARTESIAN_POINT ( 'NONE',  ( 40.31606138205700773, 42.19123852234599781, 74.30501292736987295 ) ) ;
#3977 = CARTESIAN_POINT ( 'NONE',  ( 36.98690846071097837, -11.81368208888611093, 73.30173637941818754 ) ) ;
#3978 = ORIENTED_EDGE ( 'NONE', *, *, #13595, .F. ) ;
#3979 = CARTESIAN_POINT ( 'NONE',  ( 30.81606138205697931, -4.589472609077251519, -6.350807634294812765 ) ) ;
#3980 = CARTESIAN_POINT ( 'NONE',  ( 31.56606138205707879, -39.09901169483120498, 63.57464975149190423 ) ) ;
#3981 = EDGE_CURVE ( 'NONE', #2408, #16502, #16837, .T. ) ;
#3982 = CARTESIAN_POINT ( 'NONE',  ( 31.81606138205700418, 38.19123852234599070, 72.05501292736988717 ) ) ;
#3983 = EDGE_CURVE ( 'NONE', #947, #1085, #19708, .T. ) ;
#3984 = VECTOR ( 'NONE', #12050, 1000.000000000000000 ) ;
#3985 = CIRCLE ( 'NONE', #8941, 0.7500000000000021094 ) ;
#3986 = DIRECTION ( 'NONE',  ( 0.000000000000000000, 1.000000000000000000, -2.999999999999999839E-15 ) ) ;
#3987 = CARTESIAN_POINT ( 'NONE',  ( 45.06606138205707879, -38.42645682328033985, 63.90656833300437256 ) ) ;
#3988 = CARTESIAN_POINT ( 'NONE',  ( 38.73920764526923932, -11.50384086642191050, 70.26206559358664094 ) ) ;
#3989 = CARTESIAN_POINT ( 'NONE',  ( 37.31647492878122563, -27.31368208888610027, 70.72433947564853440 ) ) ;
#3990 = ORIENTED_EDGE ( 'NONE', *, *, #3421, .F. ) ;
#3991 = CARTESIAN_POINT ( 'NONE',  ( 29.81606138205709300, -43.53621639303161572, 70.30601027268440362 ) ) ;
#3992 = CYLINDRICAL_SURFACE ( 'NONE', #24663, 0.5000000000000004441 ) ;
#3993 = ORIENTED_EDGE ( 'NONE', *, *, #17052, .T. ) ;
#3994 = ORIENTED_EDGE ( 'NONE', *, *, #7465, .F. ) ;
#3995 = CARTESIAN_POINT ( 'NONE',  ( 38.37017380507018771, -29.60384086642191193, 69.04448340153878405 ) ) ;
#3996 = EDGE_CURVE ( 'NONE', #7231, #14345, #8614, .T. ) ;
#3997 = CARTESIAN_POINT ( 'NONE',  ( 38.73920764526925353, -26.11368208888610454, 72.49843995877328950 ) ) ;
#3998 = CARTESIAN_POINT ( 'NONE',  ( 38.37017380507020192, -0.01368208888610778114, 73.71602215082116061 ) ) ;
#3999 = AXIS2_PLACEMENT_3D ( 'NONE', #7120, #14975, #22831 ) ;
#4000 = ORIENTED_EDGE ( 'NONE', *, *, #23645, .T. ) ;
#4001 = LINE ( 'NONE', #11751, #4946 ) ;
#4002 = VECTOR ( 'NONE', #21853, 1000.000000000000000 ) ;
#4003 = CARTESIAN_POINT ( 'NONE',  ( 38.37017380507018771, 0.3961591335780896284, 70.24448340153880110 ) ) ;
#4004 = CIRCLE ( 'NONE', #18821, 0.7499999999999985567 ) ;
#4005 = AXIS2_PLACEMENT_3D ( 'NONE', #19163, #17234, #25059 ) ;
#4006 =( LENGTH_UNIT ( ) NAMED_UNIT ( * ) SI_UNIT ( .MILLI., .METRE. ) );
#4007 = ORIENTED_EDGE ( 'NONE', *, *, #14159, .T. ) ;
#4008 = FACE_OUTER_BOUND ( 'NONE', #21018, .T. ) ;
#4009 = DIRECTION ( 'NONE',  ( -1.000000000000000000, 6.018531076210140067E-31, 1.734723475976804876E-16 ) ) ;
#4010 = CARTESIAN_POINT ( 'NONE',  ( 40.52078840805429394, -5.003840866421915834, 72.15350918040385864 ) ) ;
#4011 = DIRECTION ( 'NONE',  ( -1.000000000000000000, 0.000000000000000000, 0.000000000000000000 ) ) ;
#4012 = CARTESIAN_POINT ( 'NONE',  ( 39.81606138205700063, -1.054793099133682244, 61.76760556592023477 ) ) ;
#4013 = CARTESIAN_POINT ( 'NONE',  ( 39.82603832034400426, -16.31368208888610738, 72.40698646996133903 ) ) ;
#4014 = DIRECTION ( 'NONE',  ( 0.000000000000000000, -0.4425581086832455213, 0.8967398287344598984 ) ) ;
#4015 = DIRECTION ( 'NONE',  ( -1.000000000000000000, 0.000000000000000000, 0.000000000000000000 ) ) ;
#4016 = CARTESIAN_POINT ( 'NONE',  ( 33.31606138205700773, -21.26162886970023536, 44.16441745890789150 ) ) ;
#4017 = CARTESIAN_POINT ( 'NONE',  ( 36.64852494920107517, -4.203840866421910683, 71.86517103874049894 ) ) ;
#4018 = CARTESIAN_POINT ( 'NONE',  ( 43.16142150209545747, 3.549114036551906270, 6.338043885949037559 ) ) ;
#4019 = CARTESIAN_POINT ( 'NONE',  ( 36.49096545463212493, -19.51368208888610312, 71.43714994484034264 ) ) ;
#4020 = AXIS2_PLACEMENT_3D ( 'NONE', #9478, #5723, #24234 ) ;
#4021 = VECTOR ( 'NONE', #6407, 1000.000000000000000 ) ;
#4022 = DIRECTION ( 'NONE',  ( -2.574571254471601357E-15, 0.8967398287344627850, 0.4425581086832399147 ) ) ;
#4023 = CARTESIAN_POINT ( 'NONE',  ( 40.14115730948191185, -19.10384086642191193, 71.43714994484030001 ) ) ;
#4024 = DIRECTION ( 'NONE',  ( 0.000000000000000000, 0.6595716529892349245, -0.7516416929448820339 ) ) ;
#4025 = ADVANCED_FACE ( 'NONE', ( #6919 ), #24421, .F. ) ;
#4026 = CARTESIAN_POINT ( 'NONE',  ( 36.49096545463212493, -13.51368208888610489, 71.43714994484034264 ) ) ;
#4027 = ORIENTED_EDGE ( 'NONE', *, *, #24359, .F. ) ;
#4028 = CARTESIAN_POINT ( 'NONE',  ( 39.73277004305198545, -22.21368208888610951, 73.23812341099225875 ) ) ;
#4029 = ORIENTED_EDGE ( 'NONE', *, *, #24971, .T. ) ;
#4030 = CARTESIAN_POINT ( 'NONE',  ( 43.31606138205700773, -15.54379676492717621, 15.94803270339611245 ) ) ;
#4031 = CARTESIAN_POINT ( 'NONE',  ( 28.81606138205695089, 1.394403967322826121, -2.658592958638802184 ) ) ;
#4032 = CARTESIAN_POINT ( 'NONE',  ( 37.69225076346193504, -15.80384086642191299, 70.42958956619168021 ) ) ;
#4033 = ORIENTED_EDGE ( 'NONE', *, *, #3407, .T. ) ;
#4034 = ORIENTED_EDGE ( 'NONE', *, *, #22950, .T. ) ;
#4035 = CARTESIAN_POINT ( 'NONE',  ( 39.59147561631770884, -28.73147929012166202, 70.27394150260606409 ) ) ;
#4036 = DIRECTION ( 'NONE',  ( 0.000000000000000000, -0.9911113317706403691, -0.1330350631819583740 ) ) ;
#4037 = ORIENTED_EDGE ( 'NONE', *, *, #6413, .F. ) ;
#4038 = CARTESIAN_POINT ( 'NONE',  ( 36.64852494920107517, -0.2038408664219101829, 71.86517103874049894 ) ) ;
#4039 = VECTOR ( 'NONE', #8852, 1000.000000000000000 ) ;
#4040 =( LENGTH_UNIT ( ) NAMED_UNIT ( * ) SI_UNIT ( .MILLI., .METRE. ) );
#4041 = CARTESIAN_POINT ( 'NONE',  ( 36.98690846071097837, -1.813682088886107602, 73.30173637941818754 ) ) ;
#4042 = CARTESIAN_POINT ( 'NONE',  ( 41.81606138205700063, -14.36460986495925241, 36.24727600202827915 ) ) ;
#4043 = ORIENTED_EDGE ( 'NONE', *, *, #11729, .F. ) ;
#4044 = EDGE_CURVE ( 'NONE', #20593, #18694, #9123, .T. ) ;
#4045 = ORIENTED_EDGE ( 'NONE', *, *, #21435, .F. ) ;
#4046 = CARTESIAN_POINT ( 'NONE',  ( 31.81606138205700418, -34.55876147765410167, 70.30501292737000085 ) ) ;
#4047 = EDGE_CURVE ( 'NONE', #13742, #19743, #12850, .T. ) ;
#4048 = CARTESIAN_POINT ( 'NONE',  ( 43.31606138205700773, -19.92642959707777806, 24.72592537066031682 ) ) ;
#4049 = CARTESIAN_POINT ( 'NONE',  ( 37.33957961208645315, -19.80384086642191122, 69.94417936956672577 ) ) ;
#4050 = EDGE_CURVE ( 'NONE', #7938, #23852, #11309, .T. ) ;
#4051 = CARTESIAN_POINT ( 'NONE',  ( 43.81606138205700063, -27.25871422114667553, 59.79942265548595515 ) ) ;
#4052 = EDGE_CURVE ( 'NONE', #17088, #2595, #15027, .T. ) ;
#4053 = AXIS2_PLACEMENT_3D ( 'NONE', #3526, #3274, #1580 ) ;
#4054 = EDGE_CURVE ( 'NONE', #10887, #11457, #17099, .T. ) ;
#4055 = VERTEX_POINT ( 'NONE', #6794 ) ;
#4056 = CARTESIAN_POINT ( 'NONE',  ( 43.05893433410182070, 3.408565912792066221, 6.350990188909392486 ) ) ;
#4057 = CARTESIAN_POINT ( 'NONE',  ( 43.31606138205700063, 3.043703737701412226, 64.67489359404071081 ) ) ;
#4058 = ORIENTED_EDGE ( 'NONE', *, *, #4137, .T. ) ;
#4059 = CARTESIAN_POINT ( 'NONE',  ( 38.93987200065210175, -8.803840866421911215, 72.33091598616827866 ) ) ;
#4060 = CARTESIAN_POINT ( 'NONE',  ( 40.31606138205700063, 9.191238522346997897, 68.80501292736998664 ) ) ;
#4061 = ORIENTED_EDGE ( 'NONE', *, *, #2467, .F. ) ;
#4062 = AXIS2_PLACEMENT_3D ( 'NONE', #18888, #22368, #24409 ) ;
#4063 = EDGE_CURVE ( 'NONE', #17824, #3140, #3689, .T. ) ;
#4064 = DIRECTION ( 'NONE',  ( 0.000000000000000000, 0.6568589528324745297, -0.7540134720837717852 ) ) ;
#4065 = ORIENTED_EDGE ( 'NONE', *, *, #24069, .T. ) ;
#4066 = ORIENTED_EDGE ( 'NONE', *, *, #4372, .T. ) ;
#4067 = EDGE_CURVE ( 'NONE', #3225, #10628, #17265, .T. ) ;
#4068 = CARTESIAN_POINT ( 'NONE',  ( 38.31606138205700063, -29.78523130861184143, 52.92072663988442116 ) ) ;
#4069 = UNCERTAINTY_MEASURE_WITH_UNIT (LENGTH_MEASURE( 1.000000000000000082E-05 ), #4040, 'distance_accuracy_value', 'NONE');
#4070 = CARTESIAN_POINT ( 'NONE',  ( 39.31564783533280405, -10.31368208888610027, 72.03616607671141026 ) ) ;
#4071 = CIRCLE ( 'NONE', #23396, 1.000000000000000000 ) ;
#4072 = CARTESIAN_POINT ( 'NONE',  ( 37.12184278917507640, -3.513682088886100452, 71.43714994484035685 ) ) ;
#4073 = ORIENTED_EDGE ( 'NONE', *, *, #15725, .F. ) ;
#4074 = ORIENTED_EDGE ( 'NONE', *, *, #11929, .T. ) ;
#4075 = CARTESIAN_POINT ( 'NONE',  ( 39.81746892067405952, 41.67000142393845152, 79.57823623207323749 ) ) ;
#4076 = CARTESIAN_POINT ( 'NONE',  ( 33.31606138205700773, -33.36512788127014772, 60.17493381834623989 ) ) ;
#4077 = EDGE_LOOP ( 'NONE', ( #9685, #7046, #5534, #5512 ) ) ;
#4078 = PLANE ( 'NONE',  #21448 ) ;
#4079 = CARTESIAN_POINT ( 'NONE',  ( 36.80608444377001831, -18.30384086642190766, 72.40698646996135324 ) ) ;
#4080 = AXIS2_PLACEMENT_3D ( 'NONE', #20303, #18610, #953 ) ;
#4081 = LINE ( 'NONE', #21978, #15298 ) ;
#4082 = EDGE_CURVE ( 'NONE', #21871, #1577, #14643, .T. ) ;
#4083 = DIRECTION ( 'NONE',  ( -1.849283715844614702E-16, 0.8212051873014210024, 0.5706330172266920187 ) ) ;
#4084 = CARTESIAN_POINT ( 'NONE',  ( 37.89291511884476904, -21.11368208888610098, 70.26206559358661252 ) ) ;
#4085 = ORIENTED_EDGE ( 'NONE', *, *, #18873, .F. ) ;
#4086 =( GEOMETRIC_REPRESENTATION_CONTEXT ( 3 ) GLOBAL_UNCERTAINTY_ASSIGNED_CONTEXT ( ( #23888 ) ) GLOBAL_UNIT_ASSIGNED_CONTEXT ( ( #1018, #18940, #17135 ) ) REPRESENTATION_CONTEXT ( 'NONE', 'WORKASPACE' ) );
#4087 = VERTEX_POINT ( 'NONE', #7178 ) ;
#4088 = VECTOR ( 'NONE', #14601, 1000.000000000000000 ) ;
#4089 = FACE_OUTER_BOUND ( 'NONE', #12981, .T. ) ;
#4090 = CARTESIAN_POINT ( 'NONE',  ( 37.33957961208646736, -15.81368208888610916, 72.81632618279321889 ) ) ;
#4091 = LINE ( 'NONE', #2393, #22535 ) ;
#4092 = CARTESIAN_POINT ( 'NONE',  ( 33.31606138205700773, -16.77230293220685198, 77.52306850662458260 ) ) ;
#4093 = AXIS2_PLACEMENT_3D ( 'NONE', #6409, #16059, #19934 ) ;
#4094 = DIRECTION ( 'NONE',  ( 0.000000000000000000, -0.5706330172266952383, 0.8212051873014186709 ) ) ;
#4095 = CARTESIAN_POINT ( 'NONE',  ( 35.31606138205700773, 3.392460599465057403, 64.84545171350526971 ) ) ;
#4096 = AXIS2_PLACEMENT_3D ( 'NONE', #1503, #23531, #5521 ) ;
#4097 = FACE_OUTER_BOUND ( 'NONE', #18488, .T. ) ;
#4098 = CARTESIAN_POINT ( 'NONE',  ( 41.06606138205700063, -13.51824891481308910, 37.72654391001022134 ) ) ;
#4099 = ORIENTED_EDGE ( 'NONE', *, *, #4913, .F. ) ;
#4100 = EDGE_CURVE ( 'NONE', #2309, #7176, #13576, .T. ) ;
#4101 = DIRECTION ( 'NONE',  ( -1.734723475976814737E-16, 1.000000000000000000, -3.491481338843135327E-15 ) ) ;
#4102 = ORIENTED_EDGE ( 'NONE', *, *, #11819, .F. ) ;
#4103 = ORIENTED_EDGE ( 'NONE', *, *, #5014, .F. ) ;
#4104 = PRODUCT_DEFINITION_CONTEXT ( 'detailed design', #5680, 'design' ) ;
#4105 = CARTESIAN_POINT ( 'NONE',  ( 39.64521430340305841, -6.803840866421918321, 73.30173637941818754 ) ) ;
#4106 = CIRCLE ( 'NONE', #21359, 1.000000000000000888 ) ;
#4107 = ORIENTED_EDGE ( 'NONE', *, *, #1499, .F. ) ;
#4108 = DIRECTION ( 'NONE',  ( 0.000000000000000000, 2.775557561562888984E-15, 1.000000000000000000 ) ) ;
#4109 = CARTESIAN_POINT ( 'NONE',  ( 38.26194895904383486, -11.01368208888609956, 69.64448340153879258 ) ) ;
#4110 = AXIS2_PLACEMENT_3D ( 'NONE', #11177, #21088, #7042 ) ;
#4111 = CIRCLE ( 'NONE', #10303, 10.00000000000000178 ) ;
#4112 = VERTEX_POINT ( 'NONE', #23007 ) ;
#4113 = CARTESIAN_POINT ( 'NONE',  ( 36.31606138205696510, -2.780187754385557319, -4.367921789353634843 ) ) ;
#4114 = EDGE_CURVE ( 'NONE', #6859, #24693, #15194, .T. ) ;
#4115 = CARTESIAN_POINT ( 'NONE',  ( 40.55423172469004811, -16.41368208888610525, 72.05058123536544201 ) ) ;
#4116 = VECTOR ( 'NONE', #3665, 1000.000000000000000 ) ;
#4117 = DIRECTION ( 'NONE',  ( 1.849283715844614702E-16, -0.8212051873014210024, -0.5706330172266920187 ) ) ;
#4118 = DIRECTION ( 'NONE',  ( 0.000000000000000000, -0.4425581086832385824, 0.8967398287344634511 ) ) ;
#4119 = CIRCLE ( 'NONE', #3698, 1.500000000000001332 ) ;
#4120 = DIRECTION ( 'NONE',  ( 0.000000000000000000, 0.6568589528324746407, -0.7540134720837716742 ) ) ;
#4121 =( NAMED_UNIT ( * ) SI_UNIT ( $, .STERADIAN. ) SOLID_ANGLE_UNIT ( ) );
#4122 = DIRECTION ( 'NONE',  ( 2.792262043613788535E-15, -0.8967398287344627850, -0.4425581086832399147 ) ) ;
#4123 = DIRECTION ( 'NONE',  ( 0.000000000000000000, 0.8212051873014210024, 0.5706330172266920187 ) ) ;
#4124 = DIRECTION ( 'NONE',  ( 0.000000000000000000, 2.999999999999999839E-15, 1.000000000000000000 ) ) ;
#4125 = CARTESIAN_POINT ( 'NONE',  ( 38.00113996487114321, -21.91368208888610170, 72.53360434286904024 ) ) ;
#4126 = VERTEX_POINT ( 'NONE', #19027 ) ;
#4127 = AXIS2_PLACEMENT_3D ( 'NONE', #13795, #1925, #5678 ) ;
#4128 = CARTESIAN_POINT ( 'NONE',  ( 32.81606138205700773, -34.55876147765401640, 70.30501292737011454 ) ) ;
#4129 = CARTESIAN_POINT ( 'NONE',  ( 34.81606138205695800, -0.1886652901601799104, -3.819484830245897911 ) ) ;
#4130 = VERTEX_POINT ( 'NONE', #14893 ) ;
#4131 = ORIENTED_EDGE ( 'NONE', *, *, #2404, .F. ) ;
#4132 = VECTOR ( 'NONE', #24496, 1000.000000000000000 ) ;
#4133 = CARTESIAN_POINT ( 'NONE',  ( 38.37017380507018771, -21.60384086642191548, 69.04448340153878405 ) ) ;
#4134 = CARTESIAN_POINT ( 'NONE',  ( 37.60469502381300089, -23.21368208888610241, 70.49320253461758057 ) ) ;
#4135 = CARTESIAN_POINT ( 'NONE',  ( 40.14115730948191185, -28.51368208888610667, 71.32335560751958781 ) ) ;
#4136 = CARTESIAN_POINT ( 'NONE',  ( 46.81606138205697221, -3.542416608809818346, -4.744096181734387407 ) ) ;
#4137 = EDGE_CURVE ( 'NONE', #17161, #8796, #22628, .T. ) ;
#4138 = CARTESIAN_POINT ( 'NONE',  ( 37.21915885897815457, -0.2038408664219102107, 71.67976084211552745 ) ) ;
#4139 = EDGE_CURVE ( 'NONE', #15007, #21826, #25055, .T. ) ;
#4140 = PLANE ( 'NONE',  #10202 ) ;
#4141 = ORIENTED_EDGE ( 'NONE', *, *, #4374, .T. ) ;
#4142 = CARTESIAN_POINT ( 'NONE',  ( 40.31606138205700773, -7.108955154158179468, 82.62193108360246185 ) ) ;
#4143 = EDGE_CURVE ( 'NONE', #24976, #13846, #18108, .T. ) ;
#4144 = PLANE ( 'NONE',  #7558 ) ;
#4145 = CARTESIAN_POINT ( 'NONE',  ( 40.33642880535521869, -3.303840866421912548, 69.98269868914867686 ) ) ;
#4146 = CARTESIAN_POINT ( 'NONE',  ( 40.81606138205700773, 37.44123852234599781, 75.30501292736990138 ) ) ;
#4147 = CARTESIAN_POINT ( 'NONE',  ( 38.82593461698262871, -4.913682088886100807, 69.62690120949091011 ) ) ;
#4148 = DIRECTION ( 'NONE',  ( -1.000000000000000000, -1.000000000000000078E-15, 0.000000000000000000 ) ) ;
#4149 = AXIS2_PLACEMENT_3D ( 'NONE', #14931, #18796, #5151 ) ;
#4150 = CARTESIAN_POINT ( 'NONE',  ( 37.69796330110504101, -27.11368208888610098, 69.66206559358661821 ) ) ;
#4151 = AXIS2_PLACEMENT_3D ( 'NONE', #18538, #14661, #7069 ) ;
#4152 = DIRECTION ( 'NONE',  ( 0.000000000000000000, -0.6568589528324746407, 0.7540134720837716742 ) ) ;
#4153 = EDGE_CURVE ( 'NONE', #8707, #4754, #8867, .T. ) ;
#4154 = CARTESIAN_POINT ( 'NONE',  ( 36.68196826583682935, -0.003840866421911393047, 70.79240656858108593 ) ) ;
#4155 = PLANE ( 'NONE',  #12494 ) ;
#4156 = CARTESIAN_POINT ( 'NONE',  ( 39.95015449827720744, -14.61368208888610454, 70.79240656858105751 ) ) ;
#4157 = LINE ( 'NONE', #8275, #20131 ) ;
#4158 = CARTESIAN_POINT ( 'NONE',  ( 36.87297107704149823, -9.903840866421901978, 70.26145752964255564 ) ) ;
#4159 = DIRECTION ( 'NONE',  ( 0.000000000000000000, 0.7540134720837717852, 0.6568589528324745297 ) ) ;
#4160 = AXIS2_PLACEMENT_3D ( 'NONE', #24016, #12704, #6391 ) ;
#4161 = CARTESIAN_POINT ( 'NONE',  ( 39.95015449827720744, -10.61368208888610631, 70.79240656858107172 ) ) ;
#4162 = ORIENTED_EDGE ( 'NONE', *, *, #6530, .F. ) ;
#4163 = CARTESIAN_POINT ( 'NONE',  ( 36.11133435605973574, -21.61368208888610454, 72.15350918040385864 ) ) ;
#4164 = ORIENTED_EDGE ( 'NONE', *, *, #21878, .T. ) ;
#4165 = LINE ( 'NONE', #401, #3289 ) ;
#4166 = DIRECTION ( 'NONE',  ( -1.000000000000000000, 0.000000000000000000, 0.000000000000000000 ) ) ;
#4167 = AXIS2_PLACEMENT_3D ( 'NONE', #19645, #15654, #9368 ) ;
#4168 = CARTESIAN_POINT ( 'NONE',  ( 39.31564783533279694, -21.30384086642190766, 70.72433947564853440 ) ) ;
#4169 = SHAPE_REPRESENTATION ( 'Base Pivot Pin', ( #2000 ), #6728 ) ;
#4170 = ORIENTED_EDGE ( 'NONE', *, *, #10595, .F. ) ;
#4171 = ORIENTED_EDGE ( 'NONE', *, *, #14095, .T. ) ;
#4172 = CYLINDRICAL_SURFACE ( 'NONE', #10075, 1.000000000000000888 ) ;
#4173 = CARTESIAN_POINT ( 'NONE',  ( 42.68042513965293949, 2.191238522347003226, 70.30501292737000085 ) ) ;
#4174 = CARTESIAN_POINT ( 'NONE',  ( 38.37017380507018771, -25.60384086642191548, 69.04448340153878405 ) ) ;
#4175 = DIRECTION ( 'NONE',  ( -1.000000000000000000, 0.000000000000000000, 0.000000000000000000 ) ) ;
#4176 = CARTESIAN_POINT ( 'NONE',  ( 40.26954217208371034, 1.286317911113898260, 69.89063713639259845 ) ) ;
#4177 = FACE_OUTER_BOUND ( 'NONE', #16014, .T. ) ;
#4178 = ORIENTED_EDGE ( 'NONE', *, *, #14604, .F. ) ;
#4179 = ORIENTED_EDGE ( 'NONE', *, *, #3584, .F. ) ;
#4180 = CARTESIAN_POINT ( 'NONE',  ( 36.31606138205700063, 5.691238522346998785, 68.80501292736998664 ) ) ;
#4181 = CARTESIAN_POINT ( 'NONE',  ( 44.31606138205700063, -20.93319939328399926, 43.78741072286599945 ) ) ;
#4182 = EDGE_CURVE ( 'NONE', #19667, #13053, #2448, .T. ) ;
#4183 = CARTESIAN_POINT ( 'NONE',  ( 40.14115730948191185, -19.10384086642191193, 71.43714994484031422 ) ) ;
#4184 = CARTESIAN_POINT ( 'NONE',  ( 31.81606138205700418, -38.55876147765429351, 66.30501292737328356 ) ) ;
#4185 = ORIENTED_EDGE ( 'NONE', *, *, #21470, .F. ) ;
#4186 = LINE ( 'NONE', #12055, #23798 ) ;
#4187 = AXIS2_PLACEMENT_3D ( 'NONE', #4274, #2197, #17935 ) ;
#4188 = LINE ( 'NONE', #4057, #10491 ) ;
#4189 = CARTESIAN_POINT ( 'NONE',  ( 38.26194895904384197, -2.603840866421912814, 72.51602215082118619 ) ) ;
#4190 = DIRECTION ( 'NONE',  ( 0.000000000000000000, 1.000000000000000000, -3.469446951953613400E-15 ) ) ;
#4191 = VERTEX_POINT ( 'NONE', #12193 ) ;
#4192 = ORIENTED_EDGE ( 'NONE', *, *, #18873, .T. ) ;
#4193 = ORIENTED_EDGE ( 'NONE', *, *, #8608, .T. ) ;
#4194 = FACE_OUTER_BOUND ( 'NONE', #13448, .T. ) ;
#4195 = CARTESIAN_POINT ( 'NONE',  ( 39.51027997493896748, -8.513682088886101340, 71.32335560751961623 ) ) ;
#4196 = ADVANCED_FACE ( 'NONE', ( #14241 ), #14487, .T. ) ;
#4197 = EDGE_CURVE ( 'NONE', #14420, #15888, #20972, .T. ) ;
#4198 = CARTESIAN_POINT ( 'NONE',  ( 39.37952058850012804, -4.613682088886100985, 70.97781676520601479 ) ) ;
#4199 = VERTEX_POINT ( 'NONE', #17982 ) ;
#4200 = ORIENTED_EDGE ( 'NONE', *, *, #5162, .F. ) ;
#4201 = DIRECTION ( 'NONE',  ( -3.491481338843135327E-15, 1.000000000000000000, -2.999999999999999839E-15 ) ) ;
#4202 = CARTESIAN_POINT ( 'NONE',  ( 40.31606138205700773, -29.06829118875199924, 75.80501292737000085 ) ) ;
#4203 = CARTESIAN_POINT ( 'NONE',  ( 30.81606138205697931, -6.210967385200574675, -3.065230171572521645 ) ) ;
#4204 = VECTOR ( 'NONE', #22571, 1000.000000000000000 ) ;
#4205 = CARTESIAN_POINT ( 'NONE',  ( 36.49096545463212493, -10.10384086642191193, 71.32335560751963044 ) ) ;
#4206 = VECTOR ( 'NONE', #14399, 1000.000000000000000 ) ;
#4207 = EDGE_CURVE ( 'NONE', #15653, #24211, #683, .T. ) ;
#4208 = CARTESIAN_POINT ( 'NONE',  ( 40.31606138205700773, -12.97731741051367749, 21.08248588348817876 ) ) ;
#4209 = VECTOR ( 'NONE', #2819, 1000.000000000000114 ) ;
#4210 = CARTESIAN_POINT ( 'NONE',  ( 43.81606138205700063, -38.55876147765404482, 61.30501292737012164 ) ) ;
#4211 = ORIENTED_EDGE ( 'NONE', *, *, #4558, .F. ) ;
#4212 = EDGE_LOOP ( 'NONE', ( #15416, #8055, #7794, #2176 ) ) ;
#4213 = DIRECTION ( 'NONE',  ( 1.000000000000000000, 0.000000000000000000, 0.000000000000000000 ) ) ;
#4214 = CARTESIAN_POINT ( 'NONE',  ( 39.29254315202756231, -10.81368208888610205, 69.94417936956673998 ) ) ;
#4215 = EDGE_CURVE ( 'NONE', #22990, #1075, #18114, .T. ) ;
#4216 = CARTESIAN_POINT ( 'NONE',  ( 43.81606138205700063, -34.55876147765404482, 61.30501292737010743 ) ) ;
#4217 = CARTESIAN_POINT ( 'NONE',  ( 39.81606138205700063, -7.415330352220093069, 56.88974067930232081 ) ) ;
#4218 = ORIENTED_EDGE ( 'NONE', *, *, #23120, .T. ) ;
#4219 = CARTESIAN_POINT ( 'NONE',  ( 44.81606138205700063, 39.39281886181299797, 81.75501292736983316 ) ) ;
#4220 = DIRECTION ( 'NONE',  ( -2.792262043613788535E-15, 0.8967398287344627850, 0.4425581086832399147 ) ) ;
#4221 = AXIS2_PLACEMENT_3D ( 'NONE', #18915, #4872, #1258 ) ;
#4222 = LINE ( 'NONE', #19936, #3675 ) ;
#4223 = DIRECTION ( 'NONE',  ( -1.734723475976804876E-16, -3.491481338843135327E-15, -1.000000000000000000 ) ) ;
#4224 = ORIENTED_EDGE ( 'NONE', *, *, #23336, .F. ) ;
#4225 = VECTOR ( 'NONE', #11817, 1000.000000000000000 ) ;
#4226 = CARTESIAN_POINT ( 'NONE',  ( 37.31134410486515662, -21.95164459809526747, 75.30860040717502102 ) ) ;
#4227 = VERTEX_POINT ( 'NONE', #564 ) ;
#4228 = EDGE_LOOP ( 'NONE', ( #18609, #19894, #8711, #23244 ) ) ;
#4229 = CARTESIAN_POINT ( 'NONE',  ( 40.56606138205696510, -1.965028424401960461, 1.888915691893686244 ) ) ;
#4230 = CARTESIAN_POINT ( 'NONE',  ( 37.50301148336529877, -2.503840866421917166, 73.69843995877330656 ) ) ;
#4231 = ADVANCED_FACE ( 'NONE', ( #4449 ), #436, .T. ) ;
#4232 = EDGE_CURVE ( 'NONE', #10390, #2339, #4704, .T. ) ;
#4233 = EDGE_LOOP ( 'NONE', ( #10281, #1028, #23778, #3174 ) ) ;
#4234 = CIRCLE ( 'NONE', #14102, 1.000000000000000888 ) ;
#4235 = LINE ( 'NONE', #3840, #19006 ) ;
#4236 = CARTESIAN_POINT ( 'NONE',  ( 36.49096545463212493, -11.51368208888609956, 71.43714994484034264 ) ) ;
#4237 = VECTOR ( 'NONE', #22258, 1000.000000000000000 ) ;
#4238 = EDGE_CURVE ( 'NONE', #12829, #6472, #1619, .T. ) ;
#4239 = EDGE_CURVE ( 'NONE', #9789, #15078, #2497, .T. ) ;
#4240 = ORIENTED_EDGE ( 'NONE', *, *, #16024, .F. ) ;
#4241 = CARTESIAN_POINT ( 'NONE',  ( 40.31606138205700773, -19.13113579875042092, 24.60350147050422720 ) ) ;
#4242 = CIRCLE ( 'NONE', #21156, 1.500000000000000222 ) ;
#4243 = CARTESIAN_POINT ( 'NONE',  ( 39.02088643472237095, -12.91368208888610525, 69.02690120949091579 ) ) ;
#4244 = AXIS2_PLACEMENT_3D ( 'NONE', #8176, #14099, #23997 ) ;
#4245 = CARTESIAN_POINT ( 'NONE',  ( 41.81606138205700063, -9.197413316359888569, 54.67416070422748220 ) ) ;
#4246 = CARTESIAN_POINT ( 'NONE',  ( 33.10060807238558311, 3.250547983414590281, 6.144371924394154583 ) ) ;
#4247 = VECTOR ( 'NONE', #24512, 1000.000000000000000 ) ;
#4248 = ADVANCED_FACE ( 'NONE', ( #12578 ), #10372, .F. ) ;
#4249 = CARTESIAN_POINT ( 'NONE',  ( 43.31606138205700063, 4.059789041072993321, 6.339735157755647776 ) ) ;
#4250 = CARTESIAN_POINT ( 'NONE',  ( 31.81606138205700418, 38.19123852234599070, 73.05501292736988717 ) ) ;
#4251 = VECTOR ( 'NONE', #22613, 1000.000000000000114 ) ;
#4252 = DIRECTION ( 'NONE',  ( 0.000000000000000000, 2.999999999999999839E-15, 1.000000000000000000 ) ) ;
#4253 = DIRECTION ( 'NONE',  ( -2.792262043613788535E-15, 0.8967398287344627850, 0.4425581086832398592 ) ) ;
#4254 = CARTESIAN_POINT ( 'NONE',  ( 37.89291511884476904, -23.11368208888610454, 70.26206559358661252 ) ) ;
#4255 = ORIENTED_EDGE ( 'NONE', *, *, #24177, .T. ) ;
#4256 = CARTESIAN_POINT ( 'NONE',  ( 39.32240756636089429, -21.96805228052070902, 75.81313792137423491 ) ) ;
#4257 = ADVANCED_FACE ( 'NONE', ( #20409 ), #8444, .F. ) ;
#4258 = VECTOR ( 'NONE', #25137, 1000.000000000000227 ) ;
#4259 = CARTESIAN_POINT ( 'NONE',  ( 38.31606138205687984, 42.19123852234599781, 75.30501292736987295 ) ) ;
#4260 = ORIENTED_EDGE ( 'NONE', *, *, #5474, .T. ) ;
#4261 = ORIENTED_EDGE ( 'NONE', *, *, #5484, .F. ) ;
#4262 = AXIS2_PLACEMENT_3D ( 'NONE', #18101, #10114, #12305 ) ;
#4263 = CARTESIAN_POINT ( 'NONE',  ( 37.50301148336529877, -22.50384086642191761, 73.69843995877327814 ) ) ;
#4264 = AXIS2_PLACEMENT_3D ( 'NONE', #10981, #20778, #24737 ) ;
#4265 = CARTESIAN_POINT ( 'NONE',  ( 37.69796330110504101, -27.11368208888609388, 69.66206559358660400 ) ) ;
#4266 = CARTESIAN_POINT ( 'NONE',  ( 40.31606138205701484, -19.73594837544667158, 24.33996001444790025 ) ) ;
#4267 = CARTESIAN_POINT ( 'NONE',  ( 32.81606138205700773, -34.55876147765400930, 73.55501292737011454 ) ) ;
#4268 = VERTEX_POINT ( 'NONE', #8703 ) ;
#4269 = AXIS2_PLACEMENT_3D ( 'NONE', #21443, #19137, #9612 ) ;
#4270 = CARTESIAN_POINT ( 'NONE',  ( 36.31606138205700063, -29.30876147765400574, 73.55501292737010033 ) ) ;
#4271 = FACE_OUTER_BOUND ( 'NONE', #20744, .T. ) ;
#4272 = CARTESIAN_POINT ( 'NONE',  ( 39.64521430340305841, -0.8038408664219169886, 73.30173637941818754 ) ) ;
#4273 = CARTESIAN_POINT ( 'NONE',  ( 29.81606138205707168, -36.80651332587436286, 65.82119181171029254 ) ) ;
#4274 = CARTESIAN_POINT ( 'NONE',  ( 43.06606138205700063, 41.44123852234599070, 73.55501292736987295 ) ) ;
#4275 = CARTESIAN_POINT ( 'NONE',  ( 40.14115730948191185, -8.513682088886104893, 71.32335560751961623 ) ) ;
#4276 = CARTESIAN_POINT ( 'NONE',  ( 43.06606138205700063, -34.55876147765400219, 74.30501292737011454 ) ) ;
#4277 = CARTESIAN_POINT ( 'NONE',  ( 39.81746892067405952, 42.57231754924293909, 79.37823623207320622 ) ) ;
#4278 = AXIS2_PLACEMENT_3D ( 'NONE', #16749, #6459, #14444 ) ;
#4279 = CARTESIAN_POINT ( 'NONE',  ( 33.31606138205700773, 3.099306811489555891, 65.29760936252343129 ) ) ;
#4280 = AXIS2_PLACEMENT_3D ( 'NONE', #13518, #16547, #4591 ) ;
#4281 = CARTESIAN_POINT ( 'NONE',  ( 39.38009889167648936, -1.403840866421906419, 70.00779233799264034 ) ) ;
#4282 = EDGE_CURVE ( 'NONE', #19015, #5870, #21143, .T. ) ;
#4283 = DIRECTION ( 'NONE',  ( 0.000000000000000000, -2.999999999999999839E-15, -1.000000000000000000 ) ) ;
#4284 = CARTESIAN_POINT ( 'NONE',  ( 39.37952058850012804, -27.00384086642191050, 71.78268878715390144 ) ) ;
#4285 = CARTESIAN_POINT ( 'NONE',  ( 38.26194895904383486, -15.01368208888610134, 69.64448340153877837 ) ) ;
#4286 = EDGE_CURVE ( 'NONE', #10132, #16259, #11121, .T. ) ;
#4287 = DIRECTION ( 'NONE',  ( -2.792262043613788535E-15, 0.8967398287344627850, 0.4425581086832399147 ) ) ;
#4288 = PRODUCT_RELATED_PRODUCT_CATEGORY ( 'part', '', ( #10148 ) ) ;
#4289 = CARTESIAN_POINT ( 'NONE',  ( 38.37017380507018771, -11.60384086642190660, 69.64448340153879258 ) ) ;
#4290 = DIRECTION ( 'NONE',  ( -1.000000000000000000, 5.204170427930415223E-30, 1.734723475976805122E-15 ) ) ;
#4291 =( GEOMETRIC_REPRESENTATION_CONTEXT ( 3 ) GLOBAL_UNCERTAINTY_ASSIGNED_CONTEXT ( ( #21115 ) ) GLOBAL_UNIT_ASSIGNED_CONTEXT ( ( #22616, #24062, #6431 ) ) REPRESENTATION_CONTEXT ( 'NONE', 'WORKASPACE' ) );
#4292 = CARTESIAN_POINT ( 'NONE',  ( 37.33957961208646736, -9.813682088886107380, 72.81632618279323310 ) ) ;
#4293 = EDGE_LOOP ( 'NONE', ( #679, #5264, #5043, #14768 ) ) ;
#4294 = CARTESIAN_POINT ( 'NONE',  ( 36.98690846071097837, -13.81368208888610916, 73.30173637941818754 ) ) ;
#4295 = ORIENTED_EDGE ( 'NONE', *, *, #23106, .T. ) ;
#4296 = CARTESIAN_POINT ( 'NONE',  ( 30.81606138205707524, -38.42645682328038248, 63.90656833300437256 ) ) ;
#4297 = AXIS2_PLACEMENT_3D ( 'NONE', #15497, #7785, #7912 ) ;
#4298 = VECTOR ( 'NONE', #6505, 1000.000000000000227 ) ;
#4299 = CARTESIAN_POINT ( 'NONE',  ( 40.64099152588522657, -1.357181138186998925, 80.05501292737000085 ) ) ;
#4300 = CARTESIAN_POINT ( 'NONE',  ( 38.73920764526923932, -17.50384086642191406, 70.26206559358661252 ) ) ;
#4301 = ORIENTED_EDGE ( 'NONE', *, *, #7674, .F. ) ;
#4302 = ORIENTED_EDGE ( 'NONE', *, *, #7371, .F. ) ;
#4303 = LINE ( 'NONE', #280, #17492 ) ;
#4304 = EDGE_CURVE ( 'NONE', #19911, #5245, #14067, .T. ) ;
#4305 = VECTOR ( 'NONE', #6606, 1000.000000000000227 ) ;
#4306 = LINE ( 'NONE', #20006, #17403 ) ;
#4307 = CARTESIAN_POINT ( 'NONE',  ( 40.52078840805429394, -23.00384086642191761, 72.15350918040381600 ) ) ;
#4308 = DIRECTION ( 'NONE',  ( 0.000000000000000000, -0.8212051873014203363, -0.5706330172266926848 ) ) ;
#4309 = CARTESIAN_POINT ( 'NONE',  ( 37.80618814713140097, -27.91368208888610880, 73.13360434286902034 ) ) ;
#4310 = DIRECTION ( 'NONE',  ( -1.000000000000000000, -2.999999999999999839E-15, 0.000000000000000000 ) ) ;
#4311 = ORIENTED_EDGE ( 'NONE', *, *, #8829, .F. ) ;
#4312 = DIRECTION ( 'NONE',  ( 1.327674326049719602E-15, -0.4425581086832399147, 0.8967398287344627850 ) ) ;
#4313 = AXIS2_PLACEMENT_3D ( 'NONE', #12685, #24751, #22582 ) ;
#4314 = CARTESIAN_POINT ( 'NONE',  ( 30.81606138205700418, 1.142818861812999742, 83.30501292736997243 ) ) ;
#4315 = CARTESIAN_POINT ( 'NONE',  ( 38.82593461698264292, -20.70384086642191335, 73.13360434286903455 ) ) ;
#4316 = SHAPE_REPRESENTATION_RELATIONSHIP ( 'NONE' , 'NONE' ,  #7525, #21819 ) ;
#4317 = CARTESIAN_POINT ( 'NONE',  ( 35.64099152588522657, -9.607181138187000258, 80.05501292737000085 ) ) ;
#4318 = EDGE_CURVE ( 'NONE', #15787, #23679, #19912, .T. ) ;
#4319 = ORIENTED_EDGE ( 'NONE', *, *, #6414, .T. ) ;
#4320 = DIRECTION ( 'NONE',  ( -1.734723475976804876E-16, 1.000000000000000000, 0.000000000000000000 ) ) ;
#4321 = VECTOR ( 'NONE', #20645, 1000.000000000000114 ) ;
#4322 = PLANE ( 'NONE',  #6993 ) ;
#4323 = CARTESIAN_POINT ( 'NONE',  ( 39.37952058850012804, -1.003840866421912281, 71.78268878715392987 ) ) ;
#4324 = DIRECTION ( 'NONE',  ( -1.000000000000000000, -1.000000000000000078E-15, 0.000000000000000000 ) ) ;
#4325 = ORIENTED_EDGE ( 'NONE', *, *, #4714, .T. ) ;
#4326 = DIRECTION ( 'NONE',  ( -1.000000000000000000, -2.999999999999999839E-15, 0.000000000000000000 ) ) ;
#4327 = ORIENTED_EDGE ( 'NONE', *, *, #9499, .T. ) ;
#4328 = ORIENTED_EDGE ( 'NONE', *, *, #3125, .T. ) ;
#4329 = DIRECTION ( 'NONE',  ( -1.327674326049719602E-15, 0.4425581086832399147, -0.8967398287344627850 ) ) ;
#4330 = FACE_OUTER_BOUND ( 'NONE', #11440, .T. ) ;
#4331 = CARTESIAN_POINT ( 'NONE',  ( 38.37017380507020192, -8.013682088886101340, 72.51602215082118619 ) ) ;
#4332 = CARTESIAN_POINT ( 'NONE',  ( 37.21915885897815457, -25.41368208888610170, 71.08074471024441721 ) ) ;
#4333 = CARTESIAN_POINT ( 'NONE',  ( 37.60469502381300089, -3.213682088886101962, 70.49320253461759478 ) ) ;
#4334 = VERTEX_POINT ( 'NONE', #14111 ) ;
#4335 = VERTEX_POINT ( 'NONE', #21966 ) ;
#4336 = CARTESIAN_POINT ( 'NONE',  ( 32.81606138205700773, 38.19123852234599070, 72.05501292736988717 ) ) ;
#4337 = EDGE_CURVE ( 'NONE', #23131, #16929, #20031, .T. ) ;
#4338 = DIRECTION ( 'NONE',  ( 0.000000000000000000, -1.000000000000000000, 2.999999999999999839E-15 ) ) ;
#4339 = CARTESIAN_POINT ( 'NONE',  ( 43.06606138205700063, 41.44123852234595518, 61.30501292736988006 ) ) ;
#4340 = CARTESIAN_POINT ( 'NONE',  ( 37.25202387243754032, -10.40384086642191441, 72.75271321436733274 ) ) ;
#4341 = DIRECTION ( 'NONE',  ( -1.000000000000000000, 0.000000000000000000, 0.000000000000000000 ) ) ;
#4342 = DIRECTION ( 'NONE',  ( 0.000000000000000000, 2.999999999999999839E-15, 1.000000000000000000 ) ) ;
#4343 = VERTEX_POINT ( 'NONE', #7009 ) ;
#4344 = ORIENTED_EDGE ( 'NONE', *, *, #7602, .T. ) ;
#4345 = VERTEX_POINT ( 'NONE', #14733 ) ;
#4346 = DIRECTION ( 'NONE',  ( 1.000000000000000000, 2.999999999999999839E-15, 0.000000000000000000 ) ) ;
#4347 = CARTESIAN_POINT ( 'NONE',  ( 39.75915168707250302, -4.713682088886099741, 70.26145752964255564 ) ) ;
#4348 = CARTESIAN_POINT ( 'NONE',  ( 33.31606138205700773, -8.868983839943650693, 54.29715396818559725 ) ) ;
#4349 = DIRECTION ( 'NONE',  ( -1.000000000000000000, -2.999999999999999839E-15, 0.000000000000000000 ) ) ;
#4350 = DIRECTION ( 'NONE',  ( -1.000000000000000000, -2.065146995210479765E-16, 1.734723475976814737E-16 ) ) ;
#4351 = CARTESIAN_POINT ( 'NONE',  ( 33.31606138205700773, -19.47805968271055477, 24.94720442500192448 ) ) ;
#4352 = AXIS2_PLACEMENT_3D ( 'NONE', #23544, #17253, #5914 ) ;
#4353 = DIRECTION ( 'NONE',  ( -1.000000000000000000, -1.734723475976804876E-16, 1.734723475976814737E-16 ) ) ;
#4354 = FACE_OUTER_BOUND ( 'NONE', #14705, .T. ) ;
#4355 = CARTESIAN_POINT ( 'NONE',  ( 43.23147868389327897, 40.95934826813394380, 79.52109337493037344 ) ) ;
#4356 = ORIENTED_EDGE ( 'NONE', *, *, #22779, .F. ) ;
#4357 = ORIENTED_EDGE ( 'NONE', *, *, #9749, .F. ) ;
#4358 = LINE ( 'NONE', #14020, #25155 ) ;
#4359 = CARTESIAN_POINT ( 'NONE',  ( 37.50301148336529877, -6.503840866421916722, 73.69843995877330656 ) ) ;
#4360 = VERTEX_POINT ( 'NONE', #11005 ) ;
#4361 = EDGE_CURVE ( 'NONE', #13874, #22091, #13202, .T. ) ;
#4362 = CARTESIAN_POINT ( 'NONE',  ( 45.81606138205696510, -3.028410647649132592, 0.3252050635115383281 ) ) ;
#4363 = CARTESIAN_POINT ( 'NONE',  ( 36.87297107704152666, -5.713682088886105959, 72.49904802271743165 ) ) ;
#4364 = CARTESIAN_POINT ( 'NONE',  ( 46.81606138205701484, -19.34838015056928029, 26.94402965816085072 ) ) ;
#4365 = CARTESIAN_POINT ( 'NONE',  ( 35.86008812008917346, -17.51368208888610667, 71.43714994484034264 ) ) ;
#4366 = CARTESIAN_POINT ( 'NONE',  ( 43.39079911632101272, 3.095977362302465785, 6.133782536096640037 ) ) ;
#4367 = CARTESIAN_POINT ( 'NONE',  ( 40.31606138205701484, -18.91453975041205382, 24.37026150481227305 ) ) ;
#4368 = FACE_OUTER_BOUND ( 'NONE', #1587, .T. ) ;
#4369 = EDGE_CURVE ( 'NONE', #23360, #22220, #7265, .T. ) ;
#4371 = SURFACE_STYLE_USAGE ( .BOTH. , #16693 ) ;
#4370 = APPLICATION_CONTEXT ( 'automotive_design' ) ;
#4372 = EDGE_CURVE ( 'NONE', #10140, #17540, #5209, .T. ) ;
#4373 = CARTESIAN_POINT ( 'NONE',  ( 33.81606138205700063, 2.191238522347003226, 70.30501292737000085 ) ) ;
#4374 = EDGE_CURVE ( 'NONE', #7542, #13262, #24629, .T. ) ;
#4375 = DIRECTION ( 'NONE',  ( 0.000000000000000000, 0.000000000000000000, 1.000000000000000000 ) ) ;
#4376 = ADVANCED_FACE ( 'NONE', ( #24762 ), #17325, .T. ) ;
#4377 = CARTESIAN_POINT ( 'NONE',  ( 42.68042513965293949, 2.191238522347003226, 70.30501292737000085 ) ) ;
#4378 = CARTESIAN_POINT ( 'NONE',  ( 37.89291511884476904, -25.11368208888610454, 70.26206559358661252 ) ) ;
#4379 = EDGE_CURVE ( 'NONE', #19007, #18511, #14995, .T. ) ;
#4380 = ORIENTED_EDGE ( 'NONE', *, *, #8306, .T. ) ;
#4381 = CARTESIAN_POINT ( 'NONE',  ( 40.31606138205700773, -20.22026907754187164, 75.50210598695683473 ) ) ;
#4382 = LINE ( 'NONE', #12626, #24258 ) ;
#4383 = VERTEX_POINT ( 'NONE', #10883 ) ;
#4384 = VERTEX_POINT ( 'NONE', #18736 ) ;
#4385 = PRODUCT_DEFINITION_CONTEXT ( 'detailed design', #14412, 'design' ) ;
#4386 = CARTESIAN_POINT ( 'NONE',  ( 36.07789103942399578, -26.20384086642191335, 72.05058123536544201 ) ) ;
#4387 = EDGE_CURVE ( 'NONE', #3296, #5392, #4927, .T. ) ;
#4388 = PRODUCT_DEFINITION_SHAPE ( 'NONE', 'NONE',  #25496 ) ;
#4389 = CARTESIAN_POINT ( 'NONE',  ( 36.11133435605973574, 0.3863179111138967392, 72.15350918040385864 ) ) ;
#4390 = CARTESIAN_POINT ( 'NONE',  ( 46.81606138205695800, -0.7562224151693112129, -1.633662118351544734 ) ) ;
#4391 = ADVANCED_FACE ( 'NONE', ( #24886 ), #16796, .F. ) ;
#4392 = CARTESIAN_POINT ( 'NONE',  ( 41.14099152588523367, -10.60718113818700026, 93.30501292736998664 ) ) ;
#4393 = ORIENTED_EDGE ( 'NONE', *, *, #25139, .T. ) ;
#4394 = CARTESIAN_POINT ( 'NONE',  ( 40.21075434067961396, -6.485969576596928299, 82.72322597119108423 ) ) ;
#4395 = FACE_OUTER_BOUND ( 'NONE', #5321, .T. ) ;
#4396 = CARTESIAN_POINT ( 'NONE',  ( 39.12911128074872380, -5.503840866421911393, 69.06206559358666652 ) ) ;
#4397 = DIRECTION ( 'NONE',  ( -1.000000000000000000, -1.000000000000000078E-15, 0.000000000000000000 ) ) ;
#4398 = DIRECTION ( 'NONE',  ( 0.000000000000000000, -0.7540134720837717852, -0.6568589528324746407 ) ) ;
#4399 = CARTESIAN_POINT ( 'NONE',  ( 37.33957961208646736, -9.813682088886107380, 72.81632618279323310 ) ) ;
#4400 = CARTESIAN_POINT ( 'NONE',  ( 40.81606138205700773, 37.44123852234599781, 74.30501292736988717 ) ) ;
#4401 = EDGE_CURVE ( 'NONE', #24591, #828, #8634, .T. ) ;
#4402 = LINE ( 'NONE', #382, #15917 ) ;
#4403 = CARTESIAN_POINT ( 'NONE',  ( 33.31606138205700773, -27.66931681479738003, 59.51410614687260647 ) ) ;
#4404 = LINE ( 'NONE', #20115, #5273 ) ;
#4405 = CARTESIAN_POINT ( 'NONE',  ( 43.14050698234171222, 3.517279818248786327, 6.340193568624436615 ) ) ;
#4406 = CARTESIAN_POINT ( 'NONE',  ( 37.21915885897815457, -28.20384086642191335, 71.67976084211551324 ) ) ;
#4407 = CARTESIAN_POINT ( 'NONE',  ( 39.98359781491296161, -12.41368208888610525, 71.86517103874047052 ) ) ;
#4408 = PLANE ( 'NONE',  #19723 ) ;
#4409 = VECTOR ( 'NONE', #7425, 1000.000000000000000 ) ;
#4410 = CARTESIAN_POINT ( 'NONE',  ( 37.33957961208645315, -9.803840866421907663, 69.94417936956673998 ) ) ;
#4411 = DIRECTION ( 'NONE',  ( 1.000000000000000000, 0.000000000000000000, 0.000000000000000000 ) ) ;
#4412 = CIRCLE ( 'NONE', #19209, 0.2000000000000057288 ) ;
#4413 = VECTOR ( 'NONE', #8060, 1000.000000000000114 ) ;
#4414 = CARTESIAN_POINT ( 'NONE',  ( 37.25202387243752611, -13.21368208888610063, 70.00779233799262613 ) ) ;
#4415 = ORIENTED_EDGE ( 'NONE', *, *, #9517, .T. ) ;
#4416 = CARTESIAN_POINT ( 'NONE',  ( 38.26194895904383486, -15.01368208888610134, 69.04448340153878405 ) ) ;
#4417 = ORIENTED_EDGE ( 'NONE', *, *, #8727, .T. ) ;
#4418 = DIRECTION ( 'NONE',  ( 0.000000000000000000, -1.000000000000000000, 3.304235192336775512E-15 ) ) ;
#4419 = CYLINDRICAL_SURFACE ( 'NONE', #7963, 1.750000000000001998 ) ;
#4420 = CARTESIAN_POINT ( 'NONE',  ( 39.41296390513587511, -19.20384086642191335, 71.08074471024441721 ) ) ;
#4421 = VERTEX_POINT ( 'NONE', #18601 ) ;
#4422 = ORIENTED_EDGE ( 'NONE', *, *, #14978, .T. ) ;
#4423 = CARTESIAN_POINT ( 'NONE',  ( 33.81606138205700063, 15.19123852234701388, 73.80501292736995822 ) ) ;
#4424 = CARTESIAN_POINT ( 'NONE',  ( 44.71606138205697079, -3.854803714928911607, -5.706129749257958572 ) ) ;
#4425 = CARTESIAN_POINT ( 'NONE',  ( 40.55423172469004101, -25.20384086642191690, 70.70992431699446001 ) ) ;
#4426 = DIRECTION ( 'NONE',  ( 1.734723475976805122E-15, 2.999999999999999839E-15, 1.000000000000000000 ) ) ;
#4427 = CARTESIAN_POINT ( 'NONE',  ( 38.26194895904383486, -27.01368208888610312, 69.64448340153876416 ) ) ;
#4428 = ADVANCED_FACE ( 'NONE', ( #22973 ), #9340, .T. ) ;
#4429 = DIRECTION ( 'NONE',  ( 0.000000000000000000, -0.6568589528324746407, 0.7540134720837717852 ) ) ;
#4430 = EDGE_CURVE ( 'NONE', #4703, #9931, #13981, .T. ) ;
#4431 = AXIS2_PLACEMENT_3D ( 'NONE', #2972, #8802, #18454 ) ;
#4432 = VERTEX_POINT ( 'NONE', #6879 ) ;
#4433 = AXIS2_PLACEMENT_3D ( 'NONE', #8401, #4531, #16241 ) ;
#4434 = AXIS2_PLACEMENT_3D ( 'NONE', #21593, #3940, #21713 ) ;
#4435 = LINE ( 'NONE', #293, #7566 ) ;
#4436 = DIRECTION ( 'NONE',  ( 1.000000000000000000, 0.000000000000000000, 0.000000000000000000 ) ) ;
#4437 = CARTESIAN_POINT ( 'NONE',  ( 40.14115730948191185, -17.10384086642191193, 71.43714994484031422 ) ) ;
#4438 =( NAMED_UNIT ( * ) SI_UNIT ( $, .STERADIAN. ) SOLID_ANGLE_UNIT ( ) );
#4439 = LINE ( 'NONE', #4317, #10021 ) ;
#4440 = DIRECTION ( 'NONE',  ( -2.792262043613788535E-15, 0.8967398287344627850, 0.4425581086832399147 ) ) ;
#4441 = PLANE ( 'NONE',  #1231 ) ;
#4442 = CARTESIAN_POINT ( 'NONE',  ( 39.24876120206129571, 1.096159133578088696, 72.12822762946751709 ) ) ;
#4443 = DIRECTION ( 'NONE',  ( 0.000000000000000000, -0.5735764363510441610, 0.8191520442889931308 ) ) ;
#4444 = VERTEX_POINT ( 'NONE', #9088 ) ;
#4445 = DIRECTION ( 'NONE',  ( -1.849283715844614456E-16, 0.8212051873014208914, 0.5706330172266919076 ) ) ;
#4446 = ORIENTED_EDGE ( 'NONE', *, *, #23269, .T. ) ;
#4447 = VERTEX_POINT ( 'NONE', #1200 ) ;
#4448 = AXIS2_PLACEMENT_3D ( 'NONE', #6566, #8641, #12765 ) ;
#4449 = FACE_OUTER_BOUND ( 'NONE', #15155, .T. ) ;
#4450 = CYLINDRICAL_SURFACE ( 'NONE', #5529, 0.2000000000000057288 ) ;
#4451 = CARTESIAN_POINT ( 'NONE',  ( 38.26194895904383486, -3.013682088886100008, 70.24448340153877268 ) ) ;
#4452 = VECTOR ( 'NONE', #5098, 1000.000000000000227 ) ;
#4453 = VECTOR ( 'NONE', #10201, 1000.000000000000227 ) ;
#4454 = CARTESIAN_POINT ( 'NONE',  ( 38.73920764526925353, -4.113682088886099208, 72.49843995877331793 ) ) ;
#4455 = ORIENTED_EDGE ( 'NONE', *, *, #19188, .F. ) ;
#4456 = EDGE_LOOP ( 'NONE', ( #21260, #25077, #17488, #8737 ) ) ;
#4457 = DIRECTION ( 'NONE',  ( -1.000000000000000000, 0.000000000000000000, 0.000000000000000000 ) ) ;
#4458 = CARTESIAN_POINT ( 'NONE',  ( 40.81606138205700773, -6.959910619544160681, 20.07251914782758107 ) ) ;
#4459 = EDGE_LOOP ( 'NONE', ( #4141, #879, #5571, #13289, #17921, #7428, #10034, #16834, #22724, #1055, #6289 ) ) ;
#4460 = DIRECTION ( 'NONE',  ( 1.000000000000000000, -6.018531076210110289E-31, -1.734723475976804876E-16 ) ) ;
#4461 = CARTESIAN_POINT ( 'NONE',  ( 37.69796330110505522, -10.50384086642190873, 73.09843995877331224 ) ) ;
#4462 = EDGE_CURVE ( 'NONE', #1877, #5235, #16931, .T. ) ;
#4463 = ADVANCED_FACE ( 'NONE', ( #2870, #942 ), #16672, .F. ) ;
#4464 = DIRECTION ( 'NONE',  ( 0.000000000000000000, 1.000000000000000000, -2.999999999999999839E-15 ) ) ;
#4465 = EDGE_CURVE ( 'NONE', #22481, #5726, #11933, .T. ) ;
#4466 = B_SPLINE_CURVE_WITH_KNOTS ( 'NONE', 3,
 ( #6523, #8466, #18755, #10654, #4841, #10528, #589, #18624, #16299, #20315, #12470, #24525 ),
 .UNSPECIFIED., .F., .F.,
 ( 4, 2, 2, 2, 2, 4 ),
 ( 0.002960931562157818973, 0.003008429244711963331, 0.003055926927266107256, 0.003150922292374415921, 0.003340913022591033253, 0.003720894483024222380 ),
 .UNSPECIFIED. ) ;
#4467 = CARTESIAN_POINT ( 'NONE',  ( 44.81606138205700063, 35.44123852234597649, 68.30501292736990138 ) ) ;
#4468 = VERTEX_POINT ( 'NONE', #23097 ) ;
#4469 = ORIENTED_EDGE ( 'NONE', *, *, #1500, .T. ) ;
#4470 = EDGE_LOOP ( 'NONE', ( #221, #7971, #22462, #16093 ) ) ;
#4471 = CARTESIAN_POINT ( 'NONE',  ( 40.31606138205700773, 43.19123852234596939, 65.30501292736988717 ) ) ;
#4472 = CARTESIAN_POINT ( 'NONE',  ( 39.98359781491296161, -10.41368208888610347, 71.86517103874048473 ) ) ;
#4473 = CARTESIAN_POINT ( 'NONE',  ( 40.31606138205700063, 8.691238522346987239, 65.30501292736998664 ) ) ;
#4474 = DIRECTION ( 'NONE',  ( -1.271715504244016160E-15, 0.4425581086832399147, -0.8967398287344627850 ) ) ;
#4475 = VECTOR ( 'NONE', #14510, 1000.000000000000000 ) ;
#4476 = ORIENTED_EDGE ( 'NONE', *, *, #11957, .F. ) ;
#4477 = DIRECTION ( 'NONE',  ( 0.000000000000000000, 0.7540134720837717852, 0.6568589528324746407 ) ) ;
#4478 = CARTESIAN_POINT ( 'NONE',  ( 42.81606138205700063, 22.19123852234703520, 80.30501292736994401 ) ) ;
#4479 = EDGE_CURVE ( 'NONE', #15276, #874, #791, .T. ) ;
#4480 = CARTESIAN_POINT ( 'NONE',  ( 39.81746892067405952, 40.76768529863396395, 79.37823623207322044 ) ) ;
#4481 = LINE ( 'NONE', #17888, #20907 ) ;
#4482 = DIRECTION ( 'NONE',  ( -1.734723475976804876E-16, -3.491481338843135327E-15, -1.000000000000000000 ) ) ;
#4483 = ORIENTED_EDGE ( 'NONE', *, *, #13189, .T. ) ;
#4484 = ORIENTED_EDGE ( 'NONE', *, *, #14301, .F. ) ;
#4485 = CARTESIAN_POINT ( 'NONE',  ( 40.71606138205695657, 2.926944320371565045, 0.2449088955976189141 ) ) ;
#4486 = CARTESIAN_POINT ( 'NONE',  ( 40.33642880535521869, -3.303840866421912548, 69.98269868914867686 ) ) ;
#4487 = VERTEX_POINT ( 'NONE', #19363 ) ;
#4488 = ORIENTED_EDGE ( 'NONE', *, *, #10233, .T. ) ;
#4489 = DIRECTION ( 'NONE',  ( 1.000000000000000000, 0.000000000000000000, 0.000000000000000000 ) ) ;
#4490 = CARTESIAN_POINT ( 'NONE',  ( 36.80608444377001121, -7.313682088886100274, 70.35351908239860563 ) ) ;
#4491 = VECTOR ( 'NONE', #11130, 1000.000000000000000 ) ;
#4492 = DIRECTION ( 'NONE',  ( -1.000000000000000000, -3.091505625455828697E-15, -4.515976121274771690E-17 ) ) ;
#4493 = CARTESIAN_POINT ( 'NONE',  ( 36.11133435605973574, -15.61368208888610454, 72.15350918040385864 ) ) ;
#4494 = CARTESIAN_POINT ( 'NONE',  ( 32.81606138205700773, -39.60075215179220720, 69.23691647014479145 ) ) ;
#4495 = CARTESIAN_POINT ( 'NONE',  ( 43.31606138205700063, -12.87480755223282358, 20.78922580900563588 ) ) ;
#4496 = FACE_OUTER_BOUND ( 'NONE', #6721, .T. ) ;
#4497 = CARTESIAN_POINT ( 'NONE',  ( 43.06606138205700063, -38.55876147765401640, 70.30501292737012875 ) ) ;
#4498 = EDGE_CURVE ( 'NONE', #12192, #786, #15492, .T. ) ;
#4499 = CARTESIAN_POINT ( 'NONE',  ( 45.61606138205700489, 44.92314894770294131, 81.17823623207320338 ) ) ;
#4500 = LINE ( 'NONE', #4377, #9031 ) ;
#4501 = CARTESIAN_POINT ( 'NONE',  ( 37.89291511884476904, -27.11368208888610454, 70.26206559358661252 ) ) ;
#4502 = VECTOR ( 'NONE', #4022, 1000.000000000000000 ) ;
#4503 = ORIENTED_EDGE ( 'NONE', *, *, #333, .F. ) ;
#4504 = CARTESIAN_POINT ( 'NONE',  ( 40.31606138205700773, -20.48271674625588190, 75.45368821557958938 ) ) ;
#4505 = DIRECTION ( 'NONE',  ( 0.000000000000000000, 0.8967398287344635621, 0.4425581086832386379 ) ) ;
#4506 = VERTEX_POINT ( 'NONE', #5971 ) ;
#4507 = ORIENTED_EDGE ( 'NONE', *, *, #13250, .F. ) ;
#4508 = CARTESIAN_POINT ( 'NONE',  ( 36.89935272106205133, -24.40384086642191974, 73.23812341099225875 ) ) ;
#4509 = VECTOR ( 'NONE', #7727, 1000.000000000000000 ) ;
#4510 = CARTESIAN_POINT ( 'NONE',  ( 40.77203464402485622, 1.486317911113896661, 71.32335560751961623 ) ) ;
#4511 = DIRECTION ( 'NONE',  ( 0.000000000000000000, -0.5706330172266920187, 0.8212051873014210024 ) ) ;
#4512 = CIRCLE ( 'NONE', #2435, 1.100000000000000311 ) ;
#4513 = VECTOR ( 'NONE', #16714, 1000.000000000000000 ) ;
#4514 = CARTESIAN_POINT ( 'NONE',  ( 38.31606138205700063, 42.51966564709218233, 71.30501292737018559 ) ) ;
#4516 = EDGE_CURVE ( 'NONE', #3821, #131, #19612, .T. ) ;
#4515 = DIRECTION ( 'NONE',  ( 0.000000000000000000, 0.7540134720837717852, 0.6568589528324747517 ) ) ;
#4517 = ORIENTED_EDGE ( 'NONE', *, *, #24579, .F. ) ;
#4518 = DIRECTION ( 'NONE',  ( 1.000000000000000000, -0.000000000000000000, 0.000000000000000000 ) ) ;
#4519 = FACE_OUTER_BOUND ( 'NONE', #11346, .T. ) ;
#4520 = CARTESIAN_POINT ( 'NONE',  ( 40.77203464402485622, -3.103840866421913258, 71.43714994484034264 ) ) ;
#4521 = EDGE_CURVE ( 'NONE', #1537, #7878, #17314, .T. ) ;
#4522 = EDGE_CURVE ( 'NONE', #22473, #18865, #7907, .T. ) ;
#4523 = CARTESIAN_POINT ( 'NONE',  ( 38.31606138205700063, -30.30876147765399864, 75.30501292736995822 ) ) ;
#4524 = VECTOR ( 'NONE', #9145, 1000.000000000000000 ) ;
#4525 = CARTESIAN_POINT ( 'NONE',  ( 32.81606138205700773, 28.12806996228107081, 65.30501292736992980 ) ) ;
#4526 = CARTESIAN_POINT ( 'NONE',  ( 38.82593461698262871, -8.913682088886101695, 69.62690120949091011 ) ) ;
#4527 = LINE ( 'NONE', #18185, #7625 ) ;
#4528 = CARTESIAN_POINT ( 'NONE',  ( 38.82593461698262871, -26.91368208888610170, 69.62690120949091011 ) ) ;
#4529 = AXIS2_PLACEMENT_3D ( 'NONE', #12316, #6626, #20162 ) ;
#4530 = AXIS2_PLACEMENT_3D ( 'NONE', #157, #15623, #25 ) ;
#4531 = DIRECTION ( 'NONE',  ( -1.000000000000000275E-15, 0.9439899321577401858, 0.3299742535180970604 ) ) ;
#4532 = EDGE_CURVE ( 'NONE', #3879, #19656, #9968, .T. ) ;
#4533 = CARTESIAN_POINT ( 'NONE',  ( 45.81606138205695089, 1.361611432489176821, -2.592146606185703916 ) ) ;
#4534 = AXIS2_PLACEMENT_3D ( 'NONE', #10560, #14543, #2179 ) ;
#4535 = CARTESIAN_POINT ( 'NONE',  ( 37.31647492878124694, -28.30384086642191477, 72.03616607671141026 ) ) ;
#4536 = CARTESIAN_POINT ( 'NONE',  ( 38.26194895904383486, -11.01368208888609956, 69.64448340153879258 ) ) ;
#4537 = ORIENTED_EDGE ( 'NONE', *, *, #14464, .T. ) ;
#4538 = DIRECTION ( 'NONE',  ( 1.000000000000000000, 0.000000000000000000, 0.000000000000000000 ) ) ;
#4539 = VECTOR ( 'NONE', #14558, 1000.000000000000000 ) ;
#4540 = EDGE_LOOP ( 'NONE', ( #4982, #20958, #20483, #6221 ) ) ;
#4541 = CARTESIAN_POINT ( 'NONE',  ( 36.87297107704149823, -13.90384086642190908, 70.26145752964252722 ) ) ;
#4542 = CARTESIAN_POINT ( 'NONE',  ( 30.81606138205700418, 40.39281886181299797, 66.30501292737000085 ) ) ;
#4543 = B_SPLINE_CURVE_WITH_KNOTS ( 'NONE', 3,
 ( #1509, #3967, #5641, #15817 ),
 .UNSPECIFIED., .F., .F.,
 ( 4, 4 ),
 ( 0.000000000000000000, 1.000000000000000000 ),
 .UNSPECIFIED. ) ;
#4544 = CARTESIAN_POINT ( 'NONE',  ( 36.68196826583682935, -7.613682088886103649, 71.96809898377890136 ) ) ;
#4545 = EDGE_LOOP ( 'NONE', ( #11039, #7124, #17534, #14179 ) ) ;
#4546 = CARTESIAN_POINT ( 'NONE',  ( 37.50301148336529167, -15.11368208888610098, 69.06206559358665231 ) ) ;
#4547 = VERTEX_POINT ( 'NONE', #13328 ) ;
#4548 = DIRECTION ( 'NONE',  ( 1.000000000000000000, 2.065146995210479765E-16, -1.734723475976814737E-16 ) ) ;
#4549 = DIRECTION ( 'NONE',  ( 0.000000000000000000, -1.000000000000000000, 0.000000000000000000 ) ) ;
#4550 = CARTESIAN_POINT ( 'NONE',  ( 37.60469502381300799, -20.40384086642191264, 72.26730301774234988 ) ) ;
#4551 = VERTEX_POINT ( 'NONE', #1955 ) ;
#4552 = EDGE_LOOP ( 'NONE', ( #22053, #24111, #23848, #23752 ) ) ;
#4553 = DIRECTION ( 'NONE',  ( 1.000000000000000000, 0.000000000000000000, -0.000000000000000000 ) ) ;
#4554 = CARTESIAN_POINT ( 'NONE',  ( 38.41621794735363693, -36.60729675983900222, 83.30501292737011454 ) ) ;
#4555 = CARTESIAN_POINT ( 'NONE',  ( 36.98690846071097127, -21.80384086642191122, 69.45876917294175712 ) ) ;
#4556 = AXIS2_PLACEMENT_3D ( 'NONE', #21742, #12479, #6415 ) ;
#4557 = EDGE_CURVE ( 'NONE', #9294, #2245, #8036, .T. ) ;
#4558 = EDGE_CURVE ( 'NONE', #3312, #4547, #5761, .T. ) ;
#4559 = CYLINDRICAL_SURFACE ( 'NONE', #20756, 1.000000000000000888 ) ;
#4560 = CARTESIAN_POINT ( 'NONE',  ( 39.29254315202756231, -26.81368208888610027, 69.94417936956671156 ) ) ;
#4561 = DIRECTION ( 'NONE',  ( 0.9797958971132711969, -0.1642410374602840950, -0.1141266034453383288 ) ) ;
#4562 = DIRECTION ( 'NONE',  ( 1.000000000000000000, -1.011922027653136605E-30, -3.373073425510455500E-16 ) ) ;
#4563 = VERTEX_POINT ( 'NONE', #7651 ) ;
#4564 = DIRECTION ( 'NONE',  ( 1.000000000000000000, 0.000000000000000000, 0.000000000000000000 ) ) ;
#4565 = CARTESIAN_POINT ( 'NONE',  ( 35.31606138205700773, 8.791238522312193382, 67.36094597237627113 ) ) ;
#4566 = EDGE_CURVE ( 'NONE', #1711, #21638, #19744, .T. ) ;
#4567 = CARTESIAN_POINT ( 'NONE',  ( 37.33957961208645315, -11.80384086642190944, 69.94417936956672577 ) ) ;
#4568 = DIRECTION ( 'NONE',  ( 0.000000000000000000, 0.000000000000000000, 1.000000000000000000 ) ) ;
#4569 = DIRECTION ( 'NONE',  ( -1.000000000000000000, 0.000000000000000000, 0.000000000000000000 ) ) ;
#4570 = VECTOR ( 'NONE', #11563, 1000.000000000000227 ) ;
#4571 = CARTESIAN_POINT ( 'NONE',  ( 35.81606138205700063, 41.44123852234599781, 74.30501292736987295 ) ) ;
#4572 = AXIS2_PLACEMENT_3D ( 'NONE', #23641, #4326, #8185 ) ;
#4573 = CARTESIAN_POINT ( 'NONE',  ( 44.81606138205700063, 34.87886987267150118, 80.75501292736984738 ) ) ;
#4574 = CARTESIAN_POINT ( 'NONE',  ( 37.12184278917507640, -0.1038408664219107880, 71.32335560751961623 ) ) ;
#4575 = CARTESIAN_POINT ( 'NONE',  ( 36.31606138205700063, -29.30876147765400574, 73.55501292737010033 ) ) ;
#4576 = ORIENTED_EDGE ( 'NONE', *, *, #15465, .T. ) ;
#4577 = ADVANCED_FACE ( 'NONE', ( #9838 ), #5839, .T. ) ;
#4578 = PLANE ( 'NONE',  #7457 ) ;
#4579 = ORIENTED_EDGE ( 'NONE', *, *, #24838, .T. ) ;
#4580 = ORIENTED_EDGE ( 'NONE', *, *, #7183, .T. ) ;
#4581 = DIRECTION ( 'NONE',  ( -1.000000000000000000, 0.000000000000000000, 0.000000000000000000 ) ) ;
#4582 = FACE_OUTER_BOUND ( 'NONE', #13387, .T. ) ;
#4583 = CARTESIAN_POINT ( 'NONE',  ( 38.26194895904383486, -7.013682088886100452, 70.24448340153877268 ) ) ;
#4584 = CARTESIAN_POINT ( 'NONE',  ( 37.25260217561390874, -1.613682088886101651, 71.78268878715394408 ) ) ;
#4585 = ORIENTED_EDGE ( 'NONE', *, *, #5809, .T. ) ;
#4586 = ORIENTED_EDGE ( 'NONE', *, *, #22066, .F. ) ;
#4587 = CARTESIAN_POINT ( 'NONE',  ( 41.31606138205700063, 8.104266321858618838, 55.82104096753806033 ) ) ;
#4588 = LINE ( 'NONE', #12455, #19435 ) ;
#4589 = VERTEX_POINT ( 'NONE', #1698 ) ;
#4590 = CARTESIAN_POINT ( 'NONE',  ( 37.25202387243754032, -8.403840866421916189, 72.75271321436733274 ) ) ;
#4591 = DIRECTION ( 'NONE',  ( 0.000000000000000000, -0.5706330172266930179, 0.8212051873014202252 ) ) ;
#4592 = ORIENTED_EDGE ( 'NONE', *, *, #2878, .T. ) ;
#4593 = ORIENTED_EDGE ( 'NONE', *, *, #2921, .T. ) ;
#4594 = AXIS2_PLACEMENT_3D ( 'NONE', #6636, #20810, #10642 ) ;
#4595 = VERTEX_POINT ( 'NONE', #23609 ) ;
#4596 = DIRECTION ( 'NONE',  ( 3.965082230804126670E-15, -0.8967398287344626739, -0.4425581086832401922 ) ) ;
#4597 = CARTESIAN_POINT ( 'NONE',  ( 36.64852494920107517, -5.413682088886106136, 70.89533451361948835 ) ) ;
#4598 = DIRECTION ( 'NONE',  ( 1.510383499235849534E-16, 0.1218693434051499741, 0.9925461516413217611 ) ) ;
#4599 = PLANE ( 'NONE',  #9606 ) ;
#4600 = DIRECTION ( 'NONE',  ( 1.000000000000000000, 1.734723475976804876E-16, -1.734723475976814737E-16 ) ) ;
#4601 = EDGE_CURVE ( 'NONE', #3377, #9564, #3769, .T. ) ;
#4602 = LINE ( 'NONE', #18011, #14789 ) ;
#4603 = CARTESIAN_POINT ( 'NONE',  ( 30.81606138205700418, 1.392818861812999964, 84.30501292737000085 ) ) ;
#4604 = EDGE_CURVE ( 'NONE', #7039, #13966, #13821, .T. ) ;
#4605 = LINE ( 'NONE', #2400, #16058 ) ;
#4606 = EDGE_LOOP ( 'NONE', ( #25096, #21984, #5612, #12063 ) ) ;
#4607 = VERTEX_POINT ( 'NONE', #21425 ) ;
#4608 = VECTOR ( 'NONE', #13640, 1000.000000000000227 ) ;
#4609 = CARTESIAN_POINT ( 'NONE',  ( 40.26954217208371034, -26.71368208888610596, 69.89063713639254161 ) ) ;
#4610 = CARTESIAN_POINT ( 'NONE',  ( 39.24876120206128860, -20.71368208888610596, 70.63227792289245599 ) ) ;
#4611 = ORIENTED_EDGE ( 'NONE', *, *, #21436, .F. ) ;
#4612 = VERTEX_POINT ( 'NONE', #19234 ) ;
#4613 = AXIS2_PLACEMENT_3D ( 'NONE', #5567, #2067, #9570 ) ;
#4614 = DIRECTION ( 'NONE',  ( 1.000000000000000000, 0.000000000000000000, -1.734723475976814737E-16 ) ) ;
#4615 = CARTESIAN_POINT ( 'NONE',  ( 40.14115730948191185, -10.51368208888609956, 71.32335560751961623 ) ) ;
#4616 = CARTESIAN_POINT ( 'NONE',  ( 36.87297107704149823, -27.90384086642190908, 70.26145752964251301 ) ) ;
#4617 = PLANE ( 'NONE',  #13281 ) ;
#4618 = ADVANCED_FACE ( 'NONE', ( #17443 ), #21679, .T. ) ;
#4619 = CARTESIAN_POINT ( 'NONE',  ( 39.73277004305198545, -10.21368208888610773, 73.23812341099225875 ) ) ;
#4620 = CYLINDRICAL_SURFACE ( 'NONE', #18917, 1.000000000000000888 ) ;
#4621 = LINE ( 'NONE', #612, #14507 ) ;
#4622 = CARTESIAN_POINT ( 'NONE',  ( 31.91606138205695942, 0.5799492015812461876, -3.145019409304214530 ) ) ;
#4623 = CARTESIAN_POINT ( 'NONE',  ( 35.64099152588523367, 1.142818861812999742, 93.30501292736998664 ) ) ;
#4624 = FACE_OUTER_BOUND ( 'NONE', #3006, .T. ) ;
#4625 = VECTOR ( 'NONE', #22753, 1000.000000000000000 ) ;
#4626 = PLANE ( 'NONE',  #21760 ) ;
#4627 = ORIENTED_EDGE ( 'NONE', *, *, #8386, .T. ) ;
#4628 = CARTESIAN_POINT ( 'NONE',  ( 39.90994555940143584, -21.43641088028507014, 75.33526458429165018 ) ) ;
#4629 = VECTOR ( 'NONE', #12230, 1000.000000000000114 ) ;
#4630 = DIRECTION ( 'NONE',  ( -1.000000000000000000, -2.999999999999999839E-15, 0.000000000000000000 ) ) ;
#4631 = VERTEX_POINT ( 'NONE', #1832 ) ;
#4632 = EDGE_LOOP ( 'NONE', ( #6317, #8991, #6559, #306 ) ) ;
#4633 = UNCERTAINTY_MEASURE_WITH_UNIT (LENGTH_MEASURE( 1.000000000000000082E-05 ), #1771, 'distance_accuracy_value', 'NONE');
#4634 = CARTESIAN_POINT ( 'NONE',  ( 38.26194895904384197, -14.60384086642191726, 73.71602215082113219 ) ) ;
#4635 = CARTESIAN_POINT ( 'NONE',  ( 36.07789103942398867, 0.5863179111138955291, 70.70992431699450265 ) ) ;
#4636 = CARTESIAN_POINT ( 'NONE',  ( 40.81606138205700773, -31.05876147765399864, 74.30501292737010033 ) ) ;
#4637 = AXIS2_PLACEMENT_3D ( 'NONE', #1477, #13352, #21198 ) ;
#4638 = CYLINDRICAL_SURFACE ( 'NONE', #2767, 1.499999999999999778 ) ;
#4639 =( NAMED_UNIT ( * ) SI_UNIT ( $, .STERADIAN. ) SOLID_ANGLE_UNIT ( ) );
#4640 = ORIENTED_EDGE ( 'NONE', *, *, #17576, .F. ) ;
#4641 = DIRECTION ( 'NONE',  ( 0.000000000000000000, 0.6568589528324745297, -0.7540134720837717852 ) ) ;
#4642 = CARTESIAN_POINT ( 'NONE',  ( 45.81606138205700063, -33.05876147765410167, 70.30501292737000085 ) ) ;
#4643 = EDGE_CURVE ( 'NONE', #16021, #12836, #9715, .T. ) ;
#4644 = AXIS2_PLACEMENT_3D ( 'NONE', #1492, #193, #1738 ) ;
#4645 = CARTESIAN_POINT ( 'NONE',  ( 35.86008812008917346, -27.51368208888610667, 71.43714994484032843 ) ) ;
#4646 = FACE_OUTER_BOUND ( 'NONE', #21078, .T. ) ;
#4647 = DIRECTION ( 'NONE',  ( 1.000000000000000000, 0.000000000000000000, 0.000000000000000000 ) ) ;
#4648 = CARTESIAN_POINT ( 'NONE',  ( 39.82603832034400426, -6.313682088886107380, 72.40698646996135324 ) ) ;
#4649 = CARTESIAN_POINT ( 'NONE',  ( 46.81606138205705037, -30.46100403034029114, 72.05704881431049103 ) ) ;
#4650 = AXIS2_PLACEMENT_3D ( 'NONE', #15290, #5515, #15164 ) ;
#4651 = CARTESIAN_POINT ( 'NONE',  ( 39.29254315202756231, -20.81368208888610027, 69.94417936956672577 ) ) ;
#4652 = CARTESIAN_POINT ( 'NONE',  ( 39.20536636138601949, -22.02770764502952616, 75.80686379705316824 ) ) ;
#4653 = AXIS2_PLACEMENT_3D ( 'NONE', #402, #14081, #2465 ) ;
#4654 = CIRCLE ( 'NONE', #14949, 1.250000000000001110 ) ;
#4655 = DIRECTION ( 'NONE',  ( -1.000000000000000000, 6.018531076210130433E-31, 1.734723475976804876E-16 ) ) ;
#4656 = CARTESIAN_POINT ( 'NONE',  ( 38.26194895904384197, -22.60384086642191548, 72.51602215082118619 ) ) ;
#4657 = CARTESIAN_POINT ( 'NONE',  ( 37.80618814713140097, -9.913682088886107024, 73.13360434286904876 ) ) ;
#4658 = LINE ( 'NONE', #20626, #5332 ) ;
#4659 = AXIS2_PLACEMENT_3D ( 'NONE', #22191, #17962, #281 ) ;
#4660 = ORIENTED_EDGE ( 'NONE', *, *, #16719, .F. ) ;
#4661 = CARTESIAN_POINT ( 'NONE',  ( 39.29254315202757653, -8.803840866421912992, 72.81632618279323310 ) ) ;
#4662 = PLANE ( 'NONE',  #12646 ) ;
#4663 = VECTOR ( 'NONE', #23361, 1000.000000000000000 ) ;
#4664 = CARTESIAN_POINT ( 'NONE',  ( 40.14115730948191185, -4.513682088886103116, 71.32335560751961623 ) ) ;
#4665 = VERTEX_POINT ( 'NONE', #1572 ) ;
#4666 = CARTESIAN_POINT ( 'NONE',  ( 39.02088643472237095, -12.91368208888610525, 69.02690120949091579 ) ) ;
#4667 = ORIENTED_EDGE ( 'NONE', *, *, #14980, .F. ) ;
#4668 = CARTESIAN_POINT ( 'NONE',  ( 31.81606138205700418, -3.831401139557048197, 80.75501292737000369 ) ) ;
#4669 = CYLINDRICAL_SURFACE ( 'NONE', #17777, 0.7500000000000008882 ) ;
#4670 = CARTESIAN_POINT ( 'NONE',  ( 38.63098279924290068, -8.703840866421911571, 72.53360434286905445 ) ) ;
#4671 =( GEOMETRIC_REPRESENTATION_CONTEXT ( 3 ) GLOBAL_UNCERTAINTY_ASSIGNED_CONTEXT ( ( #22658 ) ) GLOBAL_UNIT_ASSIGNED_CONTEXT ( ( #18674, #22910, #8895 ) ) REPRESENTATION_CONTEXT ( 'NONE', 'WORKASPACE' ) );
#4672 = DIRECTION ( 'NONE',  ( 0.000000000000000000, 0.000000000000000000, -1.000000000000000000 ) ) ;
#4673 = ORIENTED_EDGE ( 'NONE', *, *, #18785, .F. ) ;
#4674 = CARTESIAN_POINT ( 'NONE',  ( 43.31606138205700773, -19.47805968271054766, 24.94720442500192448 ) ) ;
#4675 = CARTESIAN_POINT ( 'NONE',  ( 29.81606138205706813, -35.90867894478446232, 74.07034463014319670 ) ) ;
#4676 = ADVANCED_FACE ( 'NONE', ( #9465 ), #25394, .T. ) ;
#4677 = CARTESIAN_POINT ( 'NONE',  ( 40.55423172469004101, -23.20384086642191690, 70.70992431699450265 ) ) ;
#4678 = CIRCLE ( 'NONE', #21559, 3.000000000000002665 ) ;
#4679 = CARTESIAN_POINT ( 'NONE',  ( 31.81606138205700418, -36.55876147765400930, 73.30501292737011454 ) ) ;
#4680 = CARTESIAN_POINT ( 'NONE',  ( 38.37017380507020192, 1.986317911113890666, 73.71602215082117482 ) ) ;
#4681 = CARTESIAN_POINT ( 'NONE',  ( 34.56606138205700773, 45.04446929126260102, 82.37823623207320622 ) ) ;
#4682 = CARTESIAN_POINT ( 'NONE',  ( 43.31606138205700063, 3.043703737701412226, 64.67489359404071081 ) ) ;
#4683 = ORIENTED_EDGE ( 'NONE', *, *, #18404, .T. ) ;
#4684 = DIRECTION ( 'NONE',  ( -1.734723475976814737E-16, 0.000000000000000000, -1.000000000000000000 ) ) ;
#4685 = CARTESIAN_POINT ( 'NONE',  ( 43.81606138205700063, -34.55876147765707174, 70.30501292736873609 ) ) ;
#4686 = VECTOR ( 'NONE', #23429, 1000.000000000000227 ) ;
#4687 = CARTESIAN_POINT ( 'NONE',  ( 39.95015449827720744, -17.00384086642191406, 71.96809898377887293 ) ) ;
#4688 = CARTESIAN_POINT ( 'NONE',  ( 40.31606138205700773, -16.48551471403133206, 77.11349248448009064 ) ) ;
#4689 = ADVANCED_FACE ( 'NONE', ( #21934 ), #10600, .F. ) ;
#4690 = ADVANCED_FACE ( 'NONE', ( #531 ), #10216, .F. ) ;
#4691 = DIRECTION ( 'NONE',  ( 0.000000000000000000, 0.000000000000000000, -1.000000000000000000 ) ) ;
#4692 = ADVANCED_FACE ( 'NONE', ( #8540 ), #2591, .T. ) ;
#4693 = CIRCLE ( 'NONE', #15330, 0.2000000000000057288 ) ;
#4694 = FACE_BOUND ( 'NONE', #6589, .T. ) ;
#4695 = EDGE_CURVE ( 'NONE', #1997, #21009, #18451, .T. ) ;
#4696 = CARTESIAN_POINT ( 'NONE',  ( 38.93987200065210175, 1.196159133578088118, 72.33091598616827866 ) ) ;
#4697 = EDGE_CURVE ( 'NONE', #10390, #22220, #6597, .T. ) ;
#4698 = CARTESIAN_POINT ( 'NONE',  ( 36.41626118072728246, -20.92798318178700612, 75.89274454529751779 ) ) ;
#4699 = ORIENTED_EDGE ( 'NONE', *, *, #4143, .F. ) ;
#4700 = STYLED_ITEM ( 'NONE', ( #18368 ), #16726 ) ;
#4701 = CARTESIAN_POINT ( 'NONE',  ( 40.14115730948191185, -26.51368208888610667, 71.32335560751958781 ) ) ;
#4702 = ORIENTED_EDGE ( 'NONE', *, *, #2520, .T. ) ;
#4703 = VERTEX_POINT ( 'NONE', #20000 ) ;
#4704 = LINE ( 'NONE', #24008, #11115 ) ;
#4705 = DIRECTION ( 'NONE',  ( -1.000000000000000000, 0.000000000000000000, 0.000000000000000000 ) ) ;
#4706 = CARTESIAN_POINT ( 'NONE',  ( 39.31564783533280405, -4.313682088886102051, 72.03616607671141026 ) ) ;
#4707 = CARTESIAN_POINT ( 'NONE',  ( 38.63098279924288647, -0.9136820888861024725, 70.22690120949091863 ) ) ;
#4708 = ORIENTED_EDGE ( 'NONE', *, *, #16496, .F. ) ;
#4709 = ORIENTED_EDGE ( 'NONE', *, *, #11772, .F. ) ;
#4710 = PLANE ( 'NONE',  #5794 ) ;
#4711 = DIRECTION ( 'NONE',  ( 0.000000000000000000, -0.6568589528324746407, 0.7540134720837717852 ) ) ;
#4712 = EDGE_CURVE ( 'NONE', #6796, #6622, #18079, .T. ) ;
#4713 = CARTESIAN_POINT ( 'NONE',  ( 36.68196826583682935, -14.00384086642191228, 70.79240656858107172 ) ) ;
#4714 = EDGE_CURVE ( 'NONE', #8502, #2738, #24100, .T. ) ;
#4715 =( REPRESENTATION_RELATIONSHIP ('NONE','NONE', #17377, #14684 ) REPRESENTATION_RELATIONSHIP_WITH_TRANSFORMATION ( #1818 )SHAPE_REPRESENTATION_RELATIONSHIP( ) );
#4716 = DIRECTION ( 'NONE',  ( 1.000000000000000000, 2.999999999999999839E-15, 0.000000000000000000 ) ) ;
#4717 = PRODUCT_DEFINITION_FORMATION_WITH_SPECIFIED_SOURCE ( 'ANY', '', #11362, .NOT_KNOWN. ) ;
#4718 = CARTESIAN_POINT ( 'NONE',  ( 33.31606138205700773, -37.53049398575952722, 70.06662099985001646 ) ) ;
#4719 = VERTEX_POINT ( 'NONE', #6473 ) ;
#4720 = ORIENTED_EDGE ( 'NONE', *, *, #32, .T. ) ;
#4721 = ORIENTED_EDGE ( 'NONE', *, *, #19719, .T. ) ;
#4722 = CARTESIAN_POINT ( 'NONE',  ( 44.06606138205700063, 42.11769259596595560, 81.89079936499673806 ) ) ;
#4723 = CARTESIAN_POINT ( 'NONE',  ( 37.80618814713140097, -5.913682088886107024, 73.13360434286904876 ) ) ;
#4724 = EDGE_CURVE ( 'NONE', #19809, #4112, #4165, .T. ) ;
#4725 = AXIS2_PLACEMENT_3D ( 'NONE', #16685, #18875, #22984 ) ;
#4726 = DIRECTION ( 'NONE',  ( 0.000000000000000000, 0.7540134720837716742, 0.6568589528324746407 ) ) ;
#4727 = FACE_BOUND ( 'NONE', #15687, .T. ) ;
#4728 = DIRECTION ( 'NONE',  ( 3.965082230804126670E-15, 1.000000000000000000, -3.965082230804126670E-15 ) ) ;
#4729 = CARTESIAN_POINT ( 'NONE',  ( 44.81606138205700063, -34.55876147765401640, 70.30501292737011454 ) ) ;
#4730 = CARTESIAN_POINT ( 'NONE',  ( 37.16487936434712935, -5.549719057258167609, 82.79909873374894858 ) ) ;
#4731 = DIRECTION ( 'NONE',  ( 8.791731484610113542E-17, -0.9135454576426023099, -0.4067366430757970996 ) ) ;
#4732 = EDGE_LOOP ( 'NONE', ( #17866, #21021, #20029, #20843 ) ) ;
#4733 = ORIENTED_EDGE ( 'NONE', *, *, #2184, .F. ) ;
#4734 = CARTESIAN_POINT ( 'NONE',  ( 44.81606138205700063, 35.44123852234597649, 67.80501292736990138 ) ) ;
#4735 = CARTESIAN_POINT ( 'NONE',  ( 36.29569395875881099, -0.3038408664219164890, 72.77780686321129622 ) ) ;
#4736 = CARTESIAN_POINT ( 'NONE',  ( 39.51027997493896748, -22.51368208888609246, 71.32335560751960202 ) ) ;
#4737 = ORIENTED_EDGE ( 'NONE', *, *, #2778, .T. ) ;
#4738 = ORIENTED_EDGE ( 'NONE', *, *, #21348, .F. ) ;
#4739 = LINE ( 'NONE', #12612, #5832 ) ;
#4740 = CARTESIAN_POINT ( 'NONE',  ( 36.68196826583682935, -1.613682088886104982, 71.96809898377890136 ) ) ;
#4741 = CARTESIAN_POINT ( 'NONE',  ( 39.41296390513587511, 0.7961591335780872081, 71.08074471024443142 ) ) ;
#4742 = CARTESIAN_POINT ( 'NONE',  ( 42.96606138205694236, 5.651448314156994002, 4.532640732625139002 ) ) ;
#4743 = CARTESIAN_POINT ( 'NONE',  ( 36.29569395875879678, -9.313682088886098498, 69.98269868914869107 ) ) ;
#4744 = LINE ( 'NONE', #12618, #19308 ) ;
#4745 = DIRECTION ( 'NONE',  ( 1.000000000000000000, -1.144790849096772152E-30, 1.647482979906198098E-30 ) ) ;
#4746 = CARTESIAN_POINT ( 'NONE',  ( 33.31606138205700773, -22.22127907754186893, 75.80501292736997243 ) ) ;
#4747 = CARTESIAN_POINT ( 'NONE',  ( 45.81606138205700063, 34.92314894770293421, 79.37823623207323465 ) ) ;
#4748 = CARTESIAN_POINT ( 'NONE',  ( 43.70349364522802205, 3.546438648963166962, 6.213839566231161626 ) ) ;
#4749 = DIRECTION ( 'NONE',  ( 0.000000000000000000, 0.8212051873014210024, 0.5706330172266920187 ) ) ;
#4750 = ORIENTED_EDGE ( 'NONE', *, *, #7200, .T. ) ;
#4751 = CARTESIAN_POINT ( 'NONE',  ( 40.05426416818898616, -21.21910829294392897, 75.35475896931059481 ) ) ;
#4752 = DIRECTION ( 'NONE',  ( 0.000000000000000000, 0.5706330172266919076, -0.8212051873014208914 ) ) ;
#4753 = VERTEX_POINT ( 'NONE', #10476 ) ;
#4754 = VERTEX_POINT ( 'NONE', #12164 ) ;
#4755 = CARTESIAN_POINT ( 'NONE',  ( 36.07789103942399578, -18.20384086642191690, 72.05058123536544201 ) ) ;
#4756 = CARTESIAN_POINT ( 'NONE',  ( 40.14115730948191185, -20.51368208888609601, 71.32335560751960202 ) ) ;
#4757 = CARTESIAN_POINT ( 'NONE',  ( 42.56606138205700063, -33.77966242919868733, 58.66916295099436951 ) ) ;
#4758 = DIRECTION ( 'NONE',  ( -1.000000000000000000, 0.000000000000000000, 0.000000000000000000 ) ) ;
#4759 = CARTESIAN_POINT ( 'NONE',  ( 36.31606138205700063, -5.204193249396356968, 72.80501292736992980 ) ) ;
#4760 = ORIENTED_EDGE ( 'NONE', *, *, #19396, .F. ) ;
#4761 = CARTESIAN_POINT ( 'NONE',  ( 33.31606138205700773, 7.187001342539796944, 66.09667597968754649 ) ) ;
#4762 = DIRECTION ( 'NONE',  ( 1.000000000000000000, -0.000000000000000000, 0.000000000000000000 ) ) ;
#4763 = CARTESIAN_POINT ( 'NONE',  ( 36.36258059203031934, -27.71368208888610596, 72.86986841596734621 ) ) ;
#4764 = ORIENTED_EDGE ( 'NONE', *, *, #5065, .F. ) ;
#4765 = EDGE_CURVE ( 'NONE', #16021, #9628, #14080, .T. ) ;
#4766 = CARTESIAN_POINT ( 'NONE',  ( 36.31606138205700063, -20.22127907754186893, 75.50705395623725735 ) ) ;
#4768 = EDGE_CURVE ( 'NONE', #13664, #17658, #23623, .T. ) ;
#4767 = DIRECTION ( 'NONE',  ( 0.000000000000000000, 0.6568589528324746407, -0.7540134720837717852 ) ) ;
#4769 = CARTESIAN_POINT ( 'NONE',  ( 38.93415946300897446, 1.886317911113891244, 73.09843995877332645 ) ) ;
#4770 = CARTESIAN_POINT ( 'NONE',  ( 43.31606138205700063, -33.60910547091194900, 60.61426200347987248 ) ) ;
#4771 = CARTESIAN_POINT ( 'NONE',  ( 38.37017380507020192, -18.01368208888611022, 73.11602215082116629 ) ) ;
#4772 = CARTESIAN_POINT ( 'NONE',  ( 39.90994555940143584, -21.47565429014790794, 75.83375200144557482 ) ) ;
#4773 = LINE ( 'NONE', #10717, #17444 ) ;
#4774 = CARTESIAN_POINT ( 'NONE',  ( 37.12184278917507640, -16.10384086642191193, 71.32335560751961623 ) ) ;
#4775 = CARTESIAN_POINT ( 'NONE',  ( 36.68196826583682935, -5.613682088886105426, 71.96809898377890136 ) ) ;
#4776 = ORIENTED_EDGE ( 'NONE', *, *, #7275, .T. ) ;
#4777 = CARTESIAN_POINT ( 'NONE',  ( 40.64099152588523367, 1.832818861813001021, 88.30501292736998664 ) ) ;
#4778 = ADVANCED_FACE ( 'NONE', ( #18331 ), #6355, .T. ) ;
#4779 = VERTEX_POINT ( 'NONE', #4296 ) ;
#4780 = CARTESIAN_POINT ( 'NONE',  ( 38.93415946300896024, -3.503840866421906952, 69.66206559358663242 ) ) ;
#4781 = CARTESIAN_POINT ( 'NONE',  ( 40.05245289102396100, -29.10876147765230115, 71.40796565871902146 ) ) ;
#4782 = CARTESIAN_POINT ( 'NONE',  ( 37.33957961208646736, -7.813682088886109156, 72.81632618279323310 ) ) ;
#4783 = VERTEX_POINT ( 'NONE', #20127 ) ;
#4784 = CARTESIAN_POINT ( 'NONE',  ( 40.52078840805428683, -12.61368208888610454, 70.60699637195608602 ) ) ;
#4785 = ORIENTED_EDGE ( 'NONE', *, *, #9687, .F. ) ;
#4786 = DIRECTION ( 'NONE',  ( -1.000000000000000000, -2.999999999999999839E-15, 0.000000000000000000 ) ) ;
#4787 = CARTESIAN_POINT ( 'NONE',  ( 39.81746892067405952, 41.67000142393845152, 79.37823623207322044 ) ) ;
#4788 = CARTESIAN_POINT ( 'NONE',  ( 37.89291511884479036, -14.50384086642191228, 72.49843995877330372 ) ) ;
#4789 = FACE_OUTER_BOUND ( 'NONE', #346, .T. ) ;
#4790 = ORIENTED_EDGE ( 'NONE', *, *, #10497, .F. ) ;
#4791 = CARTESIAN_POINT ( 'NONE',  ( 3.816061382056972207, -3.863943790789065691, -7.177613496534135606 ) ) ;
#4792 = DIRECTION ( 'NONE',  ( 0.000000000000000000, 1.000000000000000000, 0.000000000000000000 ) ) ;
#4793 = CARTESIAN_POINT ( 'NONE',  ( 39.02088643472237806, -14.70384086642192045, 73.73360434286898624 ) ) ;
#4794 = FACE_OUTER_BOUND ( 'NONE', #15839, .T. ) ;
#4795 = CARTESIAN_POINT ( 'NONE',  ( 32.81606138205700773, -33.39268736607245103, 60.15578379404453813 ) ) ;
#4796 = CARTESIAN_POINT ( 'NONE',  ( 38.26194895904383486, -19.01368208888610312, 69.64448340153877837 ) ) ;
#4797 = DIRECTION ( 'NONE',  ( 0.000000000000000000, -0.4425581086832397482, 0.8967398287344628960 ) ) ;
#4798 = DIRECTION ( 'NONE',  ( 0.000000000000000000, -2.999999999999999839E-15, -1.000000000000000000 ) ) ;
#4799 = ORIENTED_EDGE ( 'NONE', *, *, #21380, .F. ) ;
#4800 = DIRECTION ( 'NONE',  ( 0.000000000000000000, 1.000000000000000000, -2.999999999999999839E-15 ) ) ;
#4801 = DIRECTION ( 'NONE',  ( 1.000000000000000000, 0.000000000000000000, -0.000000000000000000 ) ) ;
#4802 = CARTESIAN_POINT ( 'NONE',  ( 38.93415946300897446, -17.50384086642190695, 69.66206559358663242 ) ) ;
#4803 = AXIS2_PLACEMENT_3D ( 'NONE', #21321, #21081, #15651 ) ;
#4804 = DIRECTION ( 'NONE',  ( 1.000000000000000000, 0.000000000000000000, 0.000000000000000000 ) ) ;
#4805 = FACE_OUTER_BOUND ( 'NONE', #2180, .T. ) ;
#4806 = VECTOR ( 'NONE', #10198, 1000.000000000000000 ) ;
#4807 = AXIS2_PLACEMENT_3D ( 'NONE', #1567, #11132, #3389 ) ;
#4808 = DIRECTION ( 'NONE',  ( 1.734723475976805122E-15, 2.999999999999999839E-15, 1.000000000000000000 ) ) ;
#4809 = EDGE_CURVE ( 'NONE', #12932, #5707, #19729, .T. ) ;
#4810 = DIRECTION ( 'NONE',  ( -1.000000000000000078E-15, 0.9439899321577400748, 0.3299742535180970049 ) ) ;
#4811 = CARTESIAN_POINT ( 'NONE',  ( 36.64852494920107517, -24.20384086642190979, 71.86517103874047052 ) ) ;
#4812 = CARTESIAN_POINT ( 'NONE',  ( 37.31068429205633663, -21.96856463034018248, 75.80811620457531319 ) ) ;
#4813 = ORIENTED_EDGE ( 'NONE', *, *, #23388, .F. ) ;
#4814 = CARTESIAN_POINT ( 'NONE',  ( 38.26194895904383486, -27.01368208888610312, 69.64448340153876416 ) ) ;
#4815 = ORIENTED_EDGE ( 'NONE', *, *, #5363, .F. ) ;
#4816 = VERTEX_POINT ( 'NONE', #22309 ) ;
#4817 = DIRECTION ( 'NONE',  ( -1.133678928659556219E-16, 0.4425581086832399147, -0.8967398287344627850 ) ) ;
#4818 = DIRECTION ( 'NONE',  ( -1.000000000000000000, 6.018531076210110289E-31, 1.734723475976804876E-16 ) ) ;
#4819 = CARTESIAN_POINT ( 'NONE',  ( 37.12184278917507640, -28.10384086642191193, 71.32335560751960202 ) ) ;
#4820 = CARTESIAN_POINT ( 'NONE',  ( 39.02742774030101458, -29.40384086642191264, 70.49320253461758057 ) ) ;
#4821 = ORIENTED_EDGE ( 'NONE', *, *, #3421, .T. ) ;
#4822 = ORIENTED_EDGE ( 'NONE', *, *, #3960, .F. ) ;
#4823 = CARTESIAN_POINT ( 'NONE',  ( 43.31606138205698642, -7.467730535347520515, -2.778285769174305919 ) ) ;
#4824 = DIRECTION ( 'NONE',  ( -1.000000000000000000, -1.208430656372714685E-15, -2.875977885193763990E-16 ) ) ;
#4825 = ORIENTED_EDGE ( 'NONE', *, *, #16116, .F. ) ;
#4826 = CARTESIAN_POINT ( 'NONE',  ( 39.82603832034400426, -5.303840866421906775, 70.35351908239857721 ) ) ;
#4827 = EDGE_CURVE ( 'NONE', #20770, #1205, #15876, .T. ) ;
#4828 = AXIS2_PLACEMENT_3D ( 'NONE', #9703, #25379, #25121 ) ;
#4829 = AXIS2_PLACEMENT_3D ( 'NONE', #11054, #6805, #24303 ) ;
#4830 = LINE ( 'NONE', #20173, #19105 ) ;
#4831 = EDGE_CURVE ( 'NONE', #15469, #12300, #4111, .T. ) ;
#4832 = LINE ( 'NONE', #957, #14673 ) ;
#4833 = EDGE_CURVE ( 'NONE', #19940, #10213, #2712, .T. ) ;
#4834 = ORIENTED_EDGE ( 'NONE', *, *, #10977, .F. ) ;
#4835 = ORIENTED_EDGE ( 'NONE', *, *, #11953, .F. ) ;
#4836 = EDGE_CURVE ( 'NONE', #13311, #16934, #15998, .T. ) ;
#4837 = ADVANCED_FACE ( 'NONE', ( #14963 ), #9058, .T. ) ;
#4838 = ORIENTED_EDGE ( 'NONE', *, *, #23556, .F. ) ;
#4839 = DIRECTION ( 'NONE',  ( -1.000000000000000000, -3.469446951953611033E-15, 0.000000000000000000 ) ) ;
#4840 = CARTESIAN_POINT ( 'NONE',  ( 40.14115730948191185, 1.486317911113897106, 71.32335560751963044 ) ) ;
#4841 = CARTESIAN_POINT ( 'NONE',  ( 39.98436526329850693, -29.10876147765399224, 71.36840536879221020 ) ) ;
#4842 = DIRECTION ( 'NONE',  ( 0.000000000000000000, -0.3299742535180970049, 0.9439899321577400748 ) ) ;
#4843 = DIRECTION ( 'NONE',  ( 0.000000000000000000, -1.000000000000000000, 3.469446951953611033E-15 ) ) ;
#4844 = ADVANCED_FACE ( 'NONE', ( #15085 ), #8673, .T. ) ;
#4845 = AXIS2_PLACEMENT_3D ( 'NONE', #10443, #8126, #9940 ) ;
#4846 = EDGE_CURVE ( 'NONE', #2503, #12061, #24473, .T. ) ;
#4847 = DIRECTION ( 'NONE',  ( -1.000000000000000000, -2.999999999999999839E-15, 0.000000000000000000 ) ) ;
#4848 = CARTESIAN_POINT ( 'NONE',  ( 36.96379791088226341, -5.704114881462953868, 82.79260900670682588 ) ) ;
#4849 = AXIS2_PLACEMENT_3D ( 'NONE', #23107, #19507, #17201 ) ;
#4850 = VECTOR ( 'NONE', #15550, 1000.000000000000000 ) ;
#4851 = CARTESIAN_POINT ( 'NONE',  ( 40.31606138205700773, -30.30876147765401996, 69.30501292737010033 ) ) ;
#4852 = ORIENTED_EDGE ( 'NONE', *, *, #11683, .F. ) ;
#4853 = VERTEX_POINT ( 'NONE', #1165 ) ;
#4854 = CARTESIAN_POINT ( 'NONE',  ( 33.31606138205700773, 7.043113989679085307, 66.83274420321491505 ) ) ;
#4855 = CARTESIAN_POINT ( 'NONE',  ( 40.33642880535521869, 0.6961591335780878964, 69.98269868914869107 ) ) ;
#4856 = CARTESIAN_POINT ( 'NONE',  ( 43.06606138205700063, 41.44123852234599070, 73.55501292736987295 ) ) ;
#4857 = CARTESIAN_POINT ( 'NONE',  ( 39.37952058850012804, -20.61368208888610098, 70.97781676520601479 ) ) ;
#4858 = ORIENTED_EDGE ( 'NONE', *, *, #21536, .T. ) ;
#4859 = ORIENTED_EDGE ( 'NONE', *, *, #5796, .F. ) ;
#4860 = CARTESIAN_POINT ( 'NONE',  ( 38.48938833801555148, 40.69123852234599781, 72.28987726642291989 ) ) ;
#4861 = CARTESIAN_POINT ( 'NONE',  ( 39.98359781491296161, -0.4136820888861053591, 71.86517103874048473 ) ) ;
#4862 = CARTESIAN_POINT ( 'NONE',  ( 39.82603832034400426, -27.30384086642191122, 70.35351908239857721 ) ) ;
#4863 = FACE_BOUND ( 'NONE', #13578, .T. ) ;
#4864 = CARTESIAN_POINT ( 'NONE',  ( 38.37017380507020192, -6.013682088886110222, 73.71602215082116061 ) ) ;
#4865 = VECTOR ( 'NONE', #22494, 999.9999999999998863 ) ;
#4866 = EDGE_CURVE ( 'NONE', #2216, #2880, #7239, .T. ) ;
#4867 = CARTESIAN_POINT ( 'NONE',  ( 32.81606138205700773, 22.19123852234699967, 69.30501292736994401 ) ) ;
#4868 = EDGE_CURVE ( 'NONE', #17400, #973, #16503, .T. ) ;
#4869 = VECTOR ( 'NONE', #5487, 1000.000000000000227 ) ;
#4870 = PLANE ( 'NONE',  #5075 ) ;
#4871 = FACE_BOUND ( 'NONE', #2107, .T. ) ;
#4872 = DIRECTION ( 'NONE',  ( 2.497472433317076378E-15, -0.8967398287344627850, -0.4425581086832399147 ) ) ;
#4873 = CARTESIAN_POINT ( 'NONE',  ( 39.82611197195675601, -5.853481738078078145, 82.77929352097653748 ) ) ;
#4874 = LINE ( 'NONE', #9008, #312 ) ;
#4875 = AXIS2_PLACEMENT_3D ( 'NONE', #1962, #6447, #8510 ) ;
#4876 = CYLINDRICAL_SURFACE ( 'NONE', #9436, 1.500000000000001332 ) ;
#4877 = ORIENTED_EDGE ( 'NONE', *, *, #22949, .F. ) ;
#4878 = CARTESIAN_POINT ( 'NONE',  ( 38.44690133353662276, -22.22127907754186893, 75.29996292736998953 ) ) ;
#4879 = EDGE_LOOP ( 'NONE', ( #20930, #20768, #17898, #4699 ) ) ;
#4880 = VERTEX_POINT ( 'NONE', #1299 ) ;
#4881 = CARTESIAN_POINT ( 'NONE',  ( 39.73277004305197124, -19.40384086642191264, 69.52238214136768590 ) ) ;
#4882 = CIRCLE ( 'NONE', #19283, 0.2314957320545540931 ) ;
#4883 = EDGE_CURVE ( 'NONE', #2906, #22, #18827, .T. ) ;
#4884 = CARTESIAN_POINT ( 'NONE',  ( 40.14115730948191185, -22.51368208888609956, 71.32335560751960202 ) ) ;
#4885 = CARTESIAN_POINT ( 'NONE',  ( 38.31606138205700063, 38.69123852234598360, 70.30501292737018559 ) ) ;
#4886 = VECTOR ( 'NONE', #13403, 1000.000000000000000 ) ;
#4887 = CARTESIAN_POINT ( 'NONE',  ( 30.81606138205700418, 24.50429740018177682, 101.9912164131601457 ) ) ;
#4888 = ORIENTED_EDGE ( 'NONE', *, *, #7043, .F. ) ;
#4889 = CARTESIAN_POINT ( 'NONE',  ( 40.31606138205700773, -16.48551471403133206, 77.11349248448009064 ) ) ;
#4890 = CARTESIAN_POINT ( 'NONE',  ( 43.81606138205700063, 41.44123852234599070, 73.55501292736987295 ) ) ;
#4891 = CARTESIAN_POINT ( 'NONE',  ( 40.33642880535524000, -28.31368208888611093, 72.77780686321125359 ) ) ;
#4892 = VERTEX_POINT ( 'NONE', #22564 ) ;
#4893 = AXIS2_PLACEMENT_3D ( 'NONE', #3566, #3965, #25459 ) ;
#4894 = FACE_OUTER_BOUND ( 'NONE', #7906, .T. ) ;
#4895 = CARTESIAN_POINT ( 'NONE',  ( 41.31606138205700063, 2.715274261285174351, 65.05190033008260286 ) ) ;
#4896 = CARTESIAN_POINT ( 'NONE',  ( 37.25202387243752611, -3.213682088886102406, 70.00779233799264034 ) ) ;
#4897 = LINE ( 'NONE', #7087, #7167 ) ;
#4898 = CARTESIAN_POINT ( 'NONE',  ( 39.75915168707250302, -20.71368208888610241, 70.26145752964252722 ) ) ;
#4899 = AXIS2_PLACEMENT_3D ( 'NONE', #1645, #19694, #25216 ) ;
#4900 = CIRCLE ( 'NONE', #12740, 0.7500000000000041078 ) ;
#4901 = CARTESIAN_POINT ( 'NONE',  ( 45.81606138205706458, -34.55876147768182705, 70.30501292735635843 ) ) ;
#4902 = DIRECTION ( 'NONE',  ( 0.000000000000000000, -2.999999999999999839E-15, -1.000000000000000000 ) ) ;
#4903 = AXIS2_PLACEMENT_3D ( 'NONE', #15152, #16704, #3302 ) ;
#4904 = CARTESIAN_POINT ( 'NONE',  ( 37.25260217561390874, -22.00384086642191406, 70.97781676520601479 ) ) ;
#4905 = CARTESIAN_POINT ( 'NONE',  ( 36.80608444377001121, -3.313682088886100718, 70.35351908239860563 ) ) ;
#4906 = ORIENTED_EDGE ( 'NONE', *, *, #14443, .T. ) ;
#4907 = DIRECTION ( 'NONE',  ( 1.000000000000000000, 0.000000000000000000, 0.000000000000000000 ) ) ;
#4908 = ORIENTED_EDGE ( 'NONE', *, *, #20594, .T. ) ;
#4909 = EDGE_CURVE ( 'NONE', #15787, #12138, #11978, .T. ) ;
#4910 = AXIS2_PLACEMENT_3D ( 'NONE', #8470, #6528, #16190 ) ;
#4911 = CARTESIAN_POINT ( 'NONE',  ( 37.69796330110505522, -4.503840866421913169, 73.09843995877331224 ) ) ;
#4912 = DIRECTION ( 'NONE',  ( 0.000000000000000000, 0.5706330172266919076, -0.8212051873014208914 ) ) ;
#4913 = EDGE_CURVE ( 'NONE', #868, #2401, #16899, .T. ) ;
#4914 = AXIS2_PLACEMENT_3D ( 'NONE', #22390, #24547, #20584 ) ;
#4915 = CARTESIAN_POINT ( 'NONE',  ( 36.87297107704152666, -7.713682088886109511, 72.49904802271743165 ) ) ;
#4916 = ORIENTED_EDGE ( 'NONE', *, *, #2727, .T. ) ;
#4917 = CARTESIAN_POINT ( 'NONE',  ( 36.07789103942398867, -9.413682088886105248, 70.70992431699450265 ) ) ;
#4918 = ORIENTED_EDGE ( 'NONE', *, *, #2958, .T. ) ;
#4919 = DIRECTION ( 'NONE',  ( 1.000000000000000000, 1.000000000000000078E-15, 0.000000000000000000 ) ) ;
#4920 = CARTESIAN_POINT ( 'NONE',  ( 39.24876120206129571, -12.90384086642191264, 72.12822762946747446 ) ) ;
#4921 = VECTOR ( 'NONE', #11743, 1000.000000000000227 ) ;
#4922 = CARTESIAN_POINT ( 'NONE',  ( 59.50607210797845426, 32.97469880962110267, 83.30501292736985874 ) ) ;
#4923 = EDGE_LOOP ( 'NONE', ( #17633, #2511, #1354, #7095 ) ) ;
#4924 = FACE_OUTER_BOUND ( 'NONE', #3399, .T. ) ;
#4925 = CARTESIAN_POINT ( 'NONE',  ( 33.31606138205697221, -3.118133360756983663, 16.65315793475036443 ) ) ;
#4926 = CARTESIAN_POINT ( 'NONE',  ( 37.61123632939164452, -17.70384086642190979, 69.02690120949091579 ) ) ;
#4927 = CIRCLE ( 'NONE', #6166, 1.250000000000001110 ) ;
#4928 = LINE ( 'NONE', #2979, #7917 ) ;
#4929 = PRESENTATION_STYLE_ASSIGNMENT (( #16650 ) ) ;
#4930 = CARTESIAN_POINT ( 'NONE',  ( 39.38009889167650357, -18.21368208888610951, 72.75271321436731853 ) ) ;
#4931 = LINE ( 'NONE', #1311, #4321 ) ;
#4932 = VECTOR ( 'NONE', #17827, 1000.000000000000000 ) ;
#4933 = CARTESIAN_POINT ( 'NONE',  ( 32.81606138205700773, 41.44123852234596939, 66.30501292736988717 ) ) ;
#4934 = AXIS2_PLACEMENT_3D ( 'NONE', #19904, #8437, #556 ) ;
#4935 = VERTEX_POINT ( 'NONE', #6846 ) ;
#4936 = DIRECTION ( 'NONE',  ( 0.000000000000000000, -1.000000000000000000, 2.999999999999999839E-15 ) ) ;
#4937 = DIRECTION ( 'NONE',  ( 1.000000000000000000, 0.000000000000000000, 0.000000000000000000 ) ) ;
#4938 = CARTESIAN_POINT ( 'NONE',  ( 39.82603832034401137, -15.30384086642190766, 70.35351908239857721 ) ) ;
#4939 = DIRECTION ( 'NONE',  ( 0.000000000000000000, 0.000000000000000000, 1.000000000000000000 ) ) ;
#4940 = DIRECTION ( 'NONE',  ( -1.000000000000000000, 0.000000000000000000, 0.000000000000000000 ) ) ;
#4941 = CARTESIAN_POINT ( 'NONE',  ( 39.75915168707250302, -26.71368208888609530, 70.26145752964249880 ) ) ;
#4942 = DIRECTION ( 'NONE',  ( 1.836970198721029688E-16, 2.999999999999999839E-15, 1.000000000000000000 ) ) ;
#4943 = DIRECTION ( 'NONE',  ( -2.690219486203388234E-15, 0.8967398287344627850, 0.4425581086832399147 ) ) ;
#4944 = CARTESIAN_POINT ( 'NONE',  ( 37.33957961208645315, -25.80384086642190766, 69.94417936956671156 ) ) ;
#4945 = FACE_OUTER_BOUND ( 'NONE', #14844, .T. ) ;
#4946 = VECTOR ( 'NONE', #17407, 1000.000000000000114 ) ;
#4947 = CARTESIAN_POINT ( 'NONE',  ( 36.49096545463212493, -27.51368208888610312, 71.43714994484030001 ) ) ;
#4948 = ORIENTED_EDGE ( 'NONE', *, *, #21348, .T. ) ;
#4949 = ORIENTED_EDGE ( 'NONE', *, *, #2374, .F. ) ;
#4950 = DIRECTION ( 'NONE',  ( -1.000000000000000000, -1.734723475976804876E-16, 1.734723475976814737E-16 ) ) ;
#4951 = FACE_OUTER_BOUND ( 'NONE', #25329, .T. ) ;
#4952 = VECTOR ( 'NONE', #21872, 1000.000000000000000 ) ;
#4953 = CARTESIAN_POINT ( 'NONE',  ( 39.41296390513587511, 1.586317911113900081, 71.67976084211552745 ) ) ;
#4954 = B_SPLINE_CURVE_WITH_KNOTS ( 'NONE', 3,
 ( #21010, #13408, #9547, #19078, #14821, #3093, #19322, #9304, #10964, #18952 ),
 .UNSPECIFIED., .F., .F.,
 ( 4, 2, 2, 2, 4 ),
 ( 0.000000000000000000, 0.2500000000000000000, 0.5000000000000000000, 0.7500000000000000000, 1.000000000000000000 ),
 .UNSPECIFIED. ) ;
#4955 = CARTESIAN_POINT ( 'NONE',  ( 37.21915885897815457, 0.5863179111138989708, 71.08074471024443142 ) ) ;
#4956 = ORIENTED_EDGE ( 'NONE', *, *, #18759, .F. ) ;
#4957 = ORIENTED_EDGE ( 'NONE', *, *, #9293, .T. ) ;
#4958 = CYLINDRICAL_SURFACE ( 'NONE', #21578, 1.499999999999999778 ) ;
#4959 = FACE_OUTER_BOUND ( 'NONE', #22359, .T. ) ;
#4960 = EDGE_LOOP ( 'NONE', ( #9982, #2506, #76, #3173 ) ) ;
#4961 = SURFACE_STYLE_FILL_AREA ( #6513 ) ;
#4962 = CARTESIAN_POINT ( 'NONE',  ( 39.98359781491296161, -7.203840866421913347, 70.89533451361947414 ) ) ;
#4963 = CARTESIAN_POINT ( 'NONE',  ( 40.31606138205700063, 8.691238522346989015, 65.80501292736998664 ) ) ;
#4964 = EDGE_CURVE ( 'NONE', #18040, #13983, #22436, .T. ) ;
#4965 = CARTESIAN_POINT ( 'NONE',  ( 38.31606138205700063, -29.30876147765401285, 70.30501292737010033 ) ) ;
#4966 = EDGE_LOOP ( 'NONE', ( #17447, #12628, #13369, #10650 ) ) ;
#4967 = ORIENTED_EDGE ( 'NONE', *, *, #12217, .F. ) ;
#4968 = DIRECTION ( 'NONE',  ( 0.000000000000000000, 1.000000000000000000, -3.469446951953613400E-15 ) ) ;
#4969 = VECTOR ( 'NONE', #7568, 1000.000000000000227 ) ;
#4970 = CARTESIAN_POINT ( 'NONE',  ( 38.93415946300898867, 1.886317911113891022, 73.09843995877332645 ) ) ;
#4971 = CARTESIAN_POINT ( 'NONE',  ( 30.81606138205700418, -27.70293563151089700, 74.66612024218476051 ) ) ;
#4972 =( LENGTH_UNIT ( ) NAMED_UNIT ( * ) SI_UNIT ( .MILLI., .METRE. ) );
#4973 = DIRECTION ( 'NONE',  ( 0.000000000000000000, -1.000000000000000000, 2.999999999999999839E-15 ) ) ;
#4974 = CIRCLE ( 'NONE', #25113, 1.000000000000000888 ) ;
#4975 = CARTESIAN_POINT ( 'NONE',  ( 32.56606138205700773, 40.92314894770289158, 83.08534301325974525 ) ) ;
#4976 = FACE_OUTER_BOUND ( 'NONE', #24006, .T. ) ;
#4977 = DIRECTION ( 'NONE',  ( -1.000000000000000000, 1.115179377413661005E-30, 3.717264591378870232E-16 ) ) ;
#4978 = PLANE ( 'NONE',  #23783 ) ;
#4979 = ADVANCED_FACE ( 'NONE', ( #8920 ), #6722, .T. ) ;
#4980 = ADVANCED_FACE ( 'NONE', ( #3228 ), #16764, .F. ) ;
#4981 = DIRECTION ( 'NONE',  ( -1.000000000000000000, -2.751104698760144965E-15, 1.228345504986737969E-16 ) ) ;
#4982 = ORIENTED_EDGE ( 'NONE', *, *, #1221, .F. ) ;
#4983 = ORIENTED_EDGE ( 'NONE', *, *, #20373, .T. ) ;
#4984 = DIRECTION ( 'NONE',  ( 1.000000000000000000, 2.440719103442461700E-15, 1.328886038262201260E-15 ) ) ;
#4985 = DIRECTION ( 'NONE',  ( 0.000000000000000000, 1.000000000000000000, 0.000000000000000000 ) ) ;
#4986 = ADVANCED_FACE ( 'NONE', ( #14831 ), #20892, .F. ) ;
#4987 = CARTESIAN_POINT ( 'NONE',  ( 38.00113996487114321, -15.91368208888609992, 72.53360434286904024 ) ) ;
#4988 = EDGE_LOOP ( 'NONE', ( #19095, #11900 ) ) ;
#4989 = ORIENTED_EDGE ( 'NONE', *, *, #9675, .T. ) ;
#4990 = LINE ( 'NONE', #16709, #23954 ) ;
#4991 = CARTESIAN_POINT ( 'NONE',  ( 38.93415946300897446, -0.1136820888861071466, 73.09843995877331224 ) ) ;
#4992 = CARTESIAN_POINT ( 'NONE',  ( 36.87297107704149823, -25.90384086642190908, 70.26145752964251301 ) ) ;
#4993 = DIRECTION ( 'NONE',  ( -1.000000000000000000, 0.000000000000000000, 0.000000000000000000 ) ) ;
#4994 = EDGE_CURVE ( 'NONE', #8119, #9175, #19091, .T. ) ;
#4995 = CARTESIAN_POINT ( 'NONE',  ( 40.52078840805428683, -8.613682088886102761, 70.60699637195608602 ) ) ;
#4996 = CARTESIAN_POINT ( 'NONE',  ( 38.31606138205700063, -1.383222575549920119, 62.14461230196212682 ) ) ;
#4997 = CARTESIAN_POINT ( 'NONE',  ( 40.05520938202761982, -6.207949209480774222, 83.25749895850351834 ) ) ;
#4998 = DIRECTION ( 'NONE',  ( 0.000000000000000000, 1.000000000000000000, 0.000000000000000000 ) ) ;
#4999 = PLANE ( 'NONE',  #14091 ) ;
#5000 = DIRECTION ( 'NONE',  ( 0.000000000000000000, -1.000000000000000000, 6.938893903907221278E-15 ) ) ;
#5001 = LINE ( 'NONE', #12869, #11874 ) ;
#5002 = LINE ( 'NONE', #24692, #23006 ) ;
#5003 = ADVANCED_FACE ( 'NONE', ( #8799 ), #5046, .T. ) ;
#5004 = ORIENTED_EDGE ( 'NONE', *, *, #10423, .T. ) ;
#5005 = ADVANCED_FACE ( 'NONE', ( #13168 ), #3102, .T. ) ;
#5006 = LINE ( 'NONE', #17242, #2043 ) ;
#5007 = VECTOR ( 'NONE', #13679, 1000.000000000000000 ) ;
#5008 = CARTESIAN_POINT ( 'NONE',  ( 33.56606138205700773, 43.19123852234595518, 61.30501292736988006 ) ) ;
#5009 = ORIENTED_EDGE ( 'NONE', *, *, #2322, .T. ) ;
#5010 = EDGE_CURVE ( 'NONE', #6622, #17440, #23034, .T. ) ;
#5011 = ORIENTED_EDGE ( 'NONE', *, *, #21302, .T. ) ;
#5012 = CARTESIAN_POINT ( 'NONE',  ( 40.52078840805429394, -15.00384086642191583, 72.15350918040381600 ) ) ;
#5013 = ADVANCED_FACE ( 'NONE', ( #11365, #9558 ), #21525, .F. ) ;
#5014 = EDGE_CURVE ( 'NONE', #8846, #17722, #19587, .T. ) ;
#5015 = CARTESIAN_POINT ( 'NONE',  ( 39.95015449827720744, -18.61368208888610454, 70.79240656858105751 ) ) ;
#5016 = CARTESIAN_POINT ( 'NONE',  ( 46.81606138205707168, -35.90387122078352178, 69.64117576433150703 ) ) ;
#5017 = DIRECTION ( 'NONE',  ( -1.000000000000000000, -1.734723475976804876E-16, 1.734723475976814737E-16 ) ) ;
#5018 = EDGE_LOOP ( 'NONE', ( #2263, #9777, #15405, #4537 ) ) ;
#5019 = FACE_OUTER_BOUND ( 'NONE', #22381, .T. ) ;
#5020 = DIRECTION ( 'NONE',  ( 1.000000000000000000, -0.000000000000000000, 0.000000000000000000 ) ) ;
#5021 = ADVANCED_FACE ( 'NONE', ( #11615 ), #24982, .T. ) ;
#5022 = CARTESIAN_POINT ( 'NONE',  ( 36.07789103942399578, -0.2038408664219136524, 72.05058123536544201 ) ) ;
#5023 = VERTEX_POINT ( 'NONE', #21265 ) ;
#5024 = AXIS2_PLACEMENT_3D ( 'NONE', #25467, #7595, #12106 ) ;
#5025 = DIRECTION ( 'NONE',  ( -1.000000000000000000, -1.734723475976804876E-16, 1.734723475976814737E-16 ) ) ;
#5026 = CARTESIAN_POINT ( 'NONE',  ( 43.23147868389327897, 42.57231754924293909, 79.57823623207325170 ) ) ;
#5027 = CARTESIAN_POINT ( 'NONE',  ( 38.82593461698262871, -0.9136820888861022505, 69.62690120949091011 ) ) ;
#5028 = DIRECTION ( 'NONE',  ( -1.000000000000000000, 0.000000000000000000, 0.000000000000000000 ) ) ;
#5029 = VECTOR ( 'NONE', #2658, 1000.000000000000227 ) ;
#5030 = CARTESIAN_POINT ( 'NONE',  ( 38.37017380507020192, -20.01368208888610667, 73.11602215082116629 ) ) ;
#5031 = CARTESIAN_POINT ( 'NONE',  ( 2.480162969315272434E-14, -8.004447042669575296, -3.950346388939042885 ) ) ;
#5032 = EDGE_CURVE ( 'NONE', #20804, #14180, #1843, .T. ) ;
#5033 = CARTESIAN_POINT ( 'NONE',  ( 39.02742774030101458, -17.40384086642191264, 70.49320253461759478 ) ) ;
#5034 = CARTESIAN_POINT ( 'NONE',  ( 36.49096545463212493, -5.513682088886105781, 71.43714994484035685 ) ) ;
#5035 = ORIENTED_EDGE ( 'NONE', *, *, #24912, .F. ) ;
#5036 = DIRECTION ( 'NONE',  ( 1.000000000000000000, 0.000000000000000000, 0.000000000000000000 ) ) ;
#5037 = ORIENTED_EDGE ( 'NONE', *, *, #7234, .F. ) ;
#5038 = AXIS2_PLACEMENT_3D ( 'NONE', #15547, #3562, #11445 ) ;
#5039 = CARTESIAN_POINT ( 'NONE',  ( 39.75915168707251723, -4.903840866421914413, 72.49904802271740323 ) ) ;
#5040 = CARTESIAN_POINT ( 'NONE',  ( 46.81606138205705747, -33.21365173458013231, 70.96885009038120984 ) ) ;
#5041 = VECTOR ( 'NONE', #16680, 1000.000000000000000 ) ;
#5042 = CARTESIAN_POINT ( 'NONE',  ( 37.33957961208646736, -5.813682088886107380, 72.81632618279323310 ) ) ;
#5043 = ORIENTED_EDGE ( 'NONE', *, *, #7696, .F. ) ;
#5044 = CARTESIAN_POINT ( 'NONE',  ( 36.98690846071097837, -7.813682088886109156, 73.30173637941818754 ) ) ;
#5045 = EDGE_LOOP ( 'NONE', ( #7807, #23486, #23253, #13343 ) ) ;
#5046 = PLANE ( 'NONE',  #25072 ) ;
#5047 = CARTESIAN_POINT ( 'NONE',  ( 38.26194895904384197, -14.60384086642191193, 72.51602215082118619 ) ) ;
#5048 = DIRECTION ( 'NONE',  ( 1.000000000000000000, 0.000000000000000000, 0.000000000000000000 ) ) ;
#5049 = ORIENTED_EDGE ( 'NONE', *, *, #3958, .T. ) ;
#5050 = AXIS2_PLACEMENT_3D ( 'NONE', #22514, #2794, #11191 ) ;
#5051 = CARTESIAN_POINT ( 'NONE',  ( 32.56606138205700773, 43.35512946304240245, 83.12823623207320622 ) ) ;
#5052 = LINE ( 'NONE', #8679, #1384 ) ;
#5053 = CARTESIAN_POINT ( 'NONE',  ( 39.73277004305197124, -13.40384086642191619, 69.52238214136768590 ) ) ;
#5054 = AXIS2_PLACEMENT_3D ( 'NONE', #6425, #12110, #475 ) ;
#5055 = ORIENTED_EDGE ( 'NONE', *, *, #16869, .F. ) ;
#5056 = CARTESIAN_POINT ( 'NONE',  ( 38.31606138205700063, -22.22127907754186893, 75.30501292736998664 ) ) ;
#5057 = DIRECTION ( 'NONE',  ( 0.000000000000000000, 0.5706330172266920187, -0.8212051873014210024 ) ) ;
#5058 = CARTESIAN_POINT ( 'NONE',  ( 38.26194895904383486, -23.01368208888609956, 69.64448340153877837 ) ) ;
#5059 = CARTESIAN_POINT ( 'NONE',  ( 44.81606138205700063, 40.39281886181299797, 84.30501292736984453 ) ) ;
#5060 = AXIS2_PLACEMENT_3D ( 'NONE', #8855, #14763, #5231 ) ;
#5061 = DIRECTION ( 'NONE',  ( 0.000000000000000000, -2.999999999999999839E-15, -1.000000000000000000 ) ) ;
#5062 = VECTOR ( 'NONE', #25157, 1000.000000000000227 ) ;
#5063 = ADVANCED_FACE ( 'NONE', ( #23448 ), #3610, .T. ) ;
#5064 = EDGE_LOOP ( 'NONE', ( #11245, #7678, #7007, #22427 ) ) ;
#5065 = EDGE_CURVE ( 'NONE', #14420, #19848, #5939, .T. ) ;
#5066 = CARTESIAN_POINT ( 'NONE',  ( 43.06606138205700063, 42.19123852234595518, 61.30501292736988006 ) ) ;
#5067 = CARTESIAN_POINT ( 'NONE',  ( 43.81606138205700063, 2.476587234117772596, 12.62587505415466538 ) ) ;
#5068 = PRODUCT_RELATED_PRODUCT_CATEGORY ( 'part', '', ( #2305 ) ) ;
#5069 = AXIS2_PLACEMENT_3D ( 'NONE', #16132, #6363, #10347 ) ;
#5070 = CARTESIAN_POINT ( 'NONE',  ( 36.64852494920107517, -10.20384086642191157, 71.86517103874049894 ) ) ;
#5071 = SHAPE_DEFINITION_REPRESENTATION ( #15043, #17377 ) ;
#5072 = CARTESIAN_POINT ( 'NONE',  ( 36.31606138205700063, -10.66749763588700262, 14.47455635838400134 ) ) ;
#5073 = CARTESIAN_POINT ( 'NONE',  ( 37.69796330110504101, -25.11368208888609388, 69.66206559358660400 ) ) ;
#5074 = CARTESIAN_POINT ( 'NONE',  ( 35.64099152588523367, 1.392818861812999964, 93.30501292736998664 ) ) ;
#5075 = AXIS2_PLACEMENT_3D ( 'NONE', #16585, #3182, #1114 ) ;
#5076 = CARTESIAN_POINT ( 'NONE',  ( 38.26194895904384907, -24.60384086642191548, 73.11602215082115208 ) ) ;
#5077 = CARTESIAN_POINT ( 'NONE',  ( 37.42719827050449766, -22.02785702039574289, 75.80686219251248303 ) ) ;
#5078 = STYLED_ITEM ( 'NONE', ( #22792 ), #10468 ) ;
#5079 = EDGE_CURVE ( 'NONE', #15185, #4753, #17541, .T. ) ;
#5080 = CARTESIAN_POINT ( 'NONE',  ( 36.68196826583682935, -27.61368208888610809, 71.96809898377887293 ) ) ;
#5081 = ORIENTED_EDGE ( 'NONE', *, *, #25086, .T. ) ;
#5082 = ORIENTED_EDGE ( 'NONE', *, *, #9738, .T. ) ;
#5083 = CARTESIAN_POINT ( 'NONE',  ( 33.24020206407681144, 3.104049617356285040, 6.135536031321588091 ) ) ;
#5084 = VECTOR ( 'NONE', #24243, 1000.000000000000000 ) ;
#5085 = LINE ( 'NONE', #12949, #1356 ) ;
#5086 = CARTESIAN_POINT ( 'NONE',  ( 38.93987200065208754, -0.8136820888860993861, 70.42958956619168021 ) ) ;
#5087 = CARTESIAN_POINT ( 'NONE',  ( 38.37017380507020192, 1.986317911113897550, 72.51602215082118619 ) ) ;
#5088 = ORIENTED_EDGE ( 'NONE', *, *, #336, .T. ) ;
#5089 = ORIENTED_EDGE ( 'NONE', *, *, #23462, .T. ) ;
#5090 = CARTESIAN_POINT ( 'NONE',  ( 43.69896204258590444, 3.548173818309678484, 6.215045287937394747 ) ) ;
#5091 = VECTOR ( 'NONE', #14837, 1000.000000000000000 ) ;
#5092 = CYLINDRICAL_SURFACE ( 'NONE', #122, 1.500000000000000222 ) ;
#5093 = EDGE_LOOP ( 'NONE', ( #5978, #2781 ) ) ;
#5094 = FACE_OUTER_BOUND ( 'NONE', #9055, .T. ) ;
#5095 = CARTESIAN_POINT ( 'NONE',  ( 39.82603832034400426, -7.303840866421906775, 70.35351908239857721 ) ) ;
#5096 = CARTESIAN_POINT ( 'NONE',  ( 35.31606138205700773, 8.104266321858618838, 55.82104096753806033 ) ) ;
#5097 = AXIS2_PLACEMENT_3D ( 'NONE', #20522, #2855, #4684 ) ;
#5098 = DIRECTION ( 'NONE',  ( 0.000000000000000000, 0.1918498038142812112, -0.9814242980364923374 ) ) ;
#5099 = ORIENTED_EDGE ( 'NONE', *, *, #20649, .F. ) ;
#5100 = ORIENTED_EDGE ( 'NONE', *, *, #17141, .T. ) ;
#5101 = EDGE_CURVE ( 'NONE', #22885, #4880, #15222, .T. ) ;
#5102 = EDGE_LOOP ( 'NONE', ( #15672, #9611, #19295, #19136 ) ) ;
#5103 = EDGE_CURVE ( 'NONE', #1244, #13733, #5813, .T. ) ;
#5104 = DIRECTION ( 'NONE',  ( 1.493079894517851385E-15, 0.4425581086832399147, -0.8967398287344626739 ) ) ;
#5105 = PRESENTATION_LAYER_ASSIGNMENT (  '', '', ( #5123 ) ) ;
#5106 = CARTESIAN_POINT ( 'NONE',  ( 39.82603832034401847, -2.313682088886107824, 72.40698646996133903 ) ) ;
#5107 = CARTESIAN_POINT ( 'NONE',  ( 32.56606138205700773, -26.74044063519535186, 83.30501292737007191 ) ) ;
#5108 = AXIS2_PLACEMENT_3D ( 'NONE', #21005, #3348, #19194 ) ;
#5109 =( LENGTH_UNIT ( ) NAMED_UNIT ( * ) SI_UNIT ( .MILLI., .METRE. ) );
#5110 = CARTESIAN_POINT ( 'NONE',  ( 40.31606138205700773, 39.69123852234599070, 73.55501292736988717 ) ) ;
#5111 = ORIENTED_EDGE ( 'NONE', *, *, #6671, .T. ) ;
#5112 = DIRECTION ( 'NONE',  ( -1.000000000000000000, 0.000000000000000000, 0.000000000000000000 ) ) ;
#5113 = AXIS2_PLACEMENT_3D ( 'NONE', #24143, #22101, #8715 ) ;
#5114 = CARTESIAN_POINT ( 'NONE',  ( 39.31606138205700063, 42.19123852234596939, 66.30501292736988717 ) ) ;
#5115 = CARTESIAN_POINT ( 'NONE',  ( 44.81606138205700063, -22.55876147765401996, 68.80501292737008612 ) ) ;
#5116 = CARTESIAN_POINT ( 'NONE',  ( 36.36850376183099343, -6.605053338531620355, 82.70927162624322193 ) ) ;
#5117 = EDGE_CURVE ( 'NONE', #24557, #14211, #4001, .T. ) ;
#5118 = DIRECTION ( 'NONE',  ( 1.000000000000000000, 0.000000000000000000, 0.000000000000000000 ) ) ;
#5119 = ORIENTED_EDGE ( 'NONE', *, *, #22759, .F. ) ;
#5120 = VERTEX_POINT ( 'NONE', #23190 ) ;
#5121 = CARTESIAN_POINT ( 'NONE',  ( 38.31606138205700063, -5.204193249396277032, 83.05501292736992980 ) ) ;
#5122 = DIRECTION ( 'NONE',  ( 0.000000000000000000, 1.000000000000000000, -2.999999999999999839E-15 ) ) ;
#5123 = STYLED_ITEM ( 'NONE', ( #1222 ), #11987 ) ;
#5124 = CARTESIAN_POINT ( 'NONE',  ( 39.37952058850012804, -14.61368208888610098, 70.97781676520601479 ) ) ;
#5125 = ORIENTED_EDGE ( 'NONE', *, *, #5616, .F. ) ;
#5126 = ORIENTED_EDGE ( 'NONE', *, *, #18690, .T. ) ;
#5127 = PLANE ( 'NONE',  #21504 ) ;
#5128 = CARTESIAN_POINT ( 'NONE',  ( 36.64852494920107517, 0.5863179111138955291, 70.89533451361948835 ) ) ;
#5129 = CARTESIAN_POINT ( 'NONE',  ( 36.49096545463212493, -26.10384086642190482, 71.32335560751960202 ) ) ;
#5130 = AXIS2_PLACEMENT_3D ( 'NONE', #11785, #4553, #8421 ) ;
#5131 = VECTOR ( 'NONE', #2851, 999.9999999999998863 ) ;
#5132 = DIRECTION ( 'NONE',  ( 0.000000000000000000, -0.8967398287344627850, -0.4425581086832399702 ) ) ;
#5133 = AXIS2_PLACEMENT_3D ( 'NONE', #7789, #17837, #11790 ) ;
#5134 = CARTESIAN_POINT ( 'NONE',  ( 38.26194895904383486, -9.013682088886101340, 69.04448340153881247 ) ) ;
#5135 = CARTESIAN_POINT ( 'NONE',  ( 41.81606138205696510, -0.8482369431493732570, -3.067843137301039302 ) ) ;
#5136 = ORIENTED_EDGE ( 'NONE', *, *, #23684, .F. ) ;
#5137 = DIRECTION ( 'NONE',  ( 1.000000000000000000, 0.000000000000000000, 0.000000000000000000 ) ) ;
#5138 = LINE ( 'NONE', #6933, #19653 ) ;
#5139 = LINE ( 'NONE', #12749, #22298 ) ;
#5140 = DIRECTION ( 'NONE',  ( -1.734723475976804876E-16, -3.491481338843135327E-15, -1.000000000000000000 ) ) ;
#5141 = CARTESIAN_POINT ( 'NONE',  ( 41.31606138205700063, 8.104266321858618838, 55.82104096753806033 ) ) ;
#5142 = CARTESIAN_POINT ( 'NONE',  ( 43.81606138205700063, 35.92314894770294131, 80.37823623207323465 ) ) ;
#5143 = VERTEX_POINT ( 'NONE', #7623 ) ;
#5144 = CARTESIAN_POINT ( 'NONE',  ( 32.81606138205700773, 22.19123852234701388, 73.80501292736992980 ) ) ;
#5145 = PLANE ( 'NONE',  #21410 ) ;
#5146 = EDGE_LOOP ( 'NONE', ( #23125, #7873, #11574, #23348 ) ) ;
#5147 = ORIENTED_EDGE ( 'NONE', *, *, #17756, .T. ) ;
#5148 = UNCERTAINTY_MEASURE_WITH_UNIT (LENGTH_MEASURE( 1.000000000000000082E-05 ), #8304, 'distance_accuracy_value', 'NONE');
#5149 = CARTESIAN_POINT ( 'NONE',  ( 39.12911128074872380, -17.50384086642191406, 69.06206559358665231 ) ) ;
#5150 = CARTESIAN_POINT ( 'NONE',  ( 39.38009889167650357, -22.21368208888610951, 72.75271321436731853 ) ) ;
#5151 = DIRECTION ( 'NONE',  ( -1.000000000000000000, 0.000000000000000000, 0.000000000000000000 ) ) ;
#5152 = ORIENTED_EDGE ( 'NONE', *, *, #14691, .T. ) ;
#5153 = LINE ( 'NONE', #8897, #3507 ) ;
#5154 = CARTESIAN_POINT ( 'NONE',  ( 44.06606138205700063, 40.39281886181299797, 82.55501292736983032 ) ) ;
#5155 = CARTESIAN_POINT ( 'NONE',  ( 36.36258059203030513, 0.09615913357808798800, 69.89063713639259845 ) ) ;
#5156 = ORIENTED_EDGE ( 'NONE', *, *, #17368, .F. ) ;
#5157 = EDGE_CURVE ( 'NONE', #7176, #4719, #13297, .T. ) ;
#5158 = DIRECTION ( 'NONE',  ( 1.000000000000000000, 3.469446951953611033E-15, 0.000000000000000000 ) ) ;
#5159 = DIRECTION ( 'NONE',  ( 0.000000000000000000, -3.469446951953611033E-15, -1.000000000000000000 ) ) ;
#5160 = CARTESIAN_POINT ( 'NONE',  ( 36.49096545463212493, -1.513682088886105559, 71.43714994484035685 ) ) ;
#5161 = LINE ( 'NONE', #4770, #2157 ) ;
#5162 = EDGE_CURVE ( 'NONE', #16232, #24915, #3309, .T. ) ;
#5163 = ORIENTED_EDGE ( 'NONE', *, *, #10385, .F. ) ;
#5164 = CARTESIAN_POINT ( 'NONE',  ( 37.80618814713140097, -19.91368208888610525, 73.13360434286903455 ) ) ;
#5165 = EDGE_CURVE ( 'NONE', #4816, #13486, #17296, .T. ) ;
#5166 = ADVANCED_FACE ( 'NONE', ( #25104 ), #13541, .T. ) ;
#5167 = EDGE_CURVE ( 'NONE', #22981, #13614, #2866, .T. ) ;
#5168 = DIRECTION ( 'NONE',  ( -1.500536805400590970E-15, 0.6529557272876933549, 0.7573960774932753104 ) ) ;
#5169 = CARTESIAN_POINT ( 'NONE',  ( 37.79523030992096011, -5.268760358274976241, 83.30484586594928942 ) ) ;
#5170 = CARTESIAN_POINT ( 'NONE',  ( 37.31647492878124694, -18.30384086642191122, 72.03616607671141026 ) ) ;
#5171 = CARTESIAN_POINT ( 'NONE',  ( 36.64852494920107517, -3.413682088886104360, 70.89533451361948835 ) ) ;
#5172 = ORIENTED_EDGE ( 'NONE', *, *, #422, .F. ) ;
#5173 = CARTESIAN_POINT ( 'NONE',  ( 41.81606138205700063, -9.197413316359888569, 54.67416070422748220 ) ) ;
#5174 = ADVANCED_FACE ( 'NONE', ( #9314 ), #23063, .F. ) ;
#5175 = ORIENTED_EDGE ( 'NONE', *, *, #5481, .F. ) ;
#5176 = EDGE_CURVE ( 'NONE', #15661, #12889, #19344, .T. ) ;
#5177 = CARTESIAN_POINT ( 'NONE',  ( 38.93415946300896024, -5.503840866421906952, 69.66206559358663242 ) ) ;
#5178 = LINE ( 'NONE', #24726, #23399 ) ;
#5179 = CARTESIAN_POINT ( 'NONE',  ( 39.82603832034400426, -2.313682088886107380, 72.40698646996135324 ) ) ;
#5180 = ORIENTED_EDGE ( 'NONE', *, *, #250, .T. ) ;
#5181 = CARTESIAN_POINT ( 'NONE',  ( 39.73277004305198545, -10.21368208888610773, 73.23812341099225875 ) ) ;
#5182 = VERTEX_POINT ( 'NONE', #6445 ) ;
#5183 = CARTESIAN_POINT ( 'NONE',  ( 46.81606138205697221, -4.349482454670835274, -5.142398479549302515 ) ) ;
#5184 = CARTESIAN_POINT ( 'NONE',  ( 37.38336156205273397, -11.90384086642191441, 70.63227792289247020 ) ) ;
#5185 = DIRECTION ( 'NONE',  ( 1.000000000000000000, 3.197344634236645231E-31, -1.734723475976814737E-16 ) ) ;
#5186 = ORIENTED_EDGE ( 'NONE', *, *, #7384, .T. ) ;
#5187 = PLANE ( 'NONE',  #9272 ) ;
#5188 = DIRECTION ( 'NONE',  ( -1.000000000000000000, -1.734723475976804876E-16, 1.734723475976814737E-16 ) ) ;
#5189 = CARTESIAN_POINT ( 'NONE',  ( 40.55423172469004101, -15.20384086642191512, 70.70992431699450265 ) ) ;
#5190 = CARTESIAN_POINT ( 'NONE',  ( 38.18494427818247061, -22.22127907754186893, 75.29996292736998953 ) ) ;
#5191 = CARTESIAN_POINT ( 'NONE',  ( 34.06606138205700773, -39.60075215179220720, 69.23691647014479145 ) ) ;
#5192 = CARTESIAN_POINT ( 'NONE',  ( 38.93415946300897446, -22.11368208888610454, 73.09843995877329803 ) ) ;
#5193 = FACE_OUTER_BOUND ( 'NONE', #629, .T. ) ;
#5194 = PLANE ( 'NONE',  #16779 ) ;
#5195 = ORIENTED_EDGE ( 'NONE', *, *, #5617, .F. ) ;
#5196 = CARTESIAN_POINT ( 'NONE',  ( 32.81606138205700773, -27.66931681479738003, 59.51410614687260647 ) ) ;
#5197 = CARTESIAN_POINT ( 'NONE',  ( 44.81606138205700063, 34.87886987267150118, 80.75501292736991843 ) ) ;
#5198 = CARTESIAN_POINT ( 'NONE',  ( 37.33957961208645315, -9.803840866421907663, 69.94417936956673998 ) ) ;
#5199 = APPLICATION_PROTOCOL_DEFINITION ( 'draft international standard', 'automotive_design', 1998, #739 ) ;
#5200 = FACE_OUTER_BOUND ( 'NONE', #18200, .T. ) ;
#5201 = CARTESIAN_POINT ( 'NONE',  ( 38.26194895904383486, -27.01368208888610312, 69.64448340153876416 ) ) ;
#5202 =( REPRESENTATION_RELATIONSHIP ('NONE','NONE', #17377, #8505 ) REPRESENTATION_RELATIONSHIP_WITH_TRANSFORMATION ( #7896 )SHAPE_REPRESENTATION_RELATIONSHIP( ) );
#5203 = DIRECTION ( 'NONE',  ( -1.000000000000000000, 0.000000000000000000, 0.000000000000000000 ) ) ;
#5204 = CARTESIAN_POINT ( 'NONE',  ( 37.80618814713138676, -23.70384086642190979, 69.62690120949091011 ) ) ;
#5205 = CARTESIAN_POINT ( 'NONE',  ( 37.09309150775561648, -5.616495718819777494, 83.30222173984805067 ) ) ;
#5206 = CARTESIAN_POINT ( 'NONE',  ( 38.37017380507020192, -26.01368208888611022, 73.11602215082115208 ) ) ;
#5207 = ORIENTED_EDGE ( 'NONE', *, *, #25128, .T. ) ;
#5208 = VERTEX_POINT ( 'NONE', #24192 ) ;
#5209 = LINE ( 'NONE', #22720, #21793 ) ;
#5210 = DIRECTION ( 'NONE',  ( 0.000000000000000000, 0.3299742535180963943, -0.9439899321577402969 ) ) ;
#5211 = CARTESIAN_POINT ( 'NONE',  ( 37.12184278917507640, 0.4863179111138996036, 71.43714994484035685 ) ) ;
#5212 = ORIENTED_EDGE ( 'NONE', *, *, #20832, .T. ) ;
#5213 = EDGE_CURVE ( 'NONE', #8578, #20287, #14425, .T. ) ;
#5214 = ORIENTED_EDGE ( 'NONE', *, *, #6903, .T. ) ;
#5215 = LINE ( 'NONE', #15000, #17896 ) ;
#5216 = CARTESIAN_POINT ( 'NONE',  ( 44.06606138205700063, 47.04446929126260102, 81.37823623207319201 ) ) ;
#5217 = VERTEX_POINT ( 'NONE', #12250 ) ;
#5218 = CARTESIAN_POINT ( 'NONE',  ( 37.25202387243754032, -2.403840866421914413, 72.75271321436733274 ) ) ;
#5219 = EDGE_CURVE ( 'NONE', #16943, #723, #2470, .T. ) ;
#5220 = DIRECTION ( 'NONE',  ( 0.000000000000000000, -0.3299742535180970049, 0.9439899321577400748 ) ) ;
#5221 = LINE ( 'NONE', #13085, #15128 ) ;
#5222 = EDGE_LOOP ( 'NONE', ( #1126, #12846, #10725, #7105 ) ) ;
#5223 = ORIENTED_EDGE ( 'NONE', *, *, #20043, .F. ) ;
#5224 = CIRCLE ( 'NONE', #14282, 1.249999999999995115 ) ;
#5225 = DIRECTION ( 'NONE',  ( 0.000000000000000000, 1.000000000000000000, -2.999999999999999839E-15 ) ) ;
#5226 = CARTESIAN_POINT ( 'NONE',  ( 37.25202387243752611, 0.7863179111138978161, 70.00779233799264034 ) ) ;
#5227 = CARTESIAN_POINT ( 'NONE',  ( 37.33957961208645315, -27.80384086642191122, 69.94417936956671156 ) ) ;
#5228 = PLANE ( 'NONE',  #16560 ) ;
#5229 = EDGE_LOOP ( 'NONE', ( #23204, #15684, #19840, #7719 ) ) ;
#5230 = CARTESIAN_POINT ( 'NONE',  ( 44.31606138205700063, 9.733755362416909307, 68.18201966341686671 ) ) ;
#5231 = DIRECTION ( 'NONE',  ( -1.000000000000000000, 0.000000000000000000, 0.000000000000000000 ) ) ;
#5232 = FACE_BOUND ( 'NONE', #5527, .T. ) ;
#5233 = DIRECTION ( 'NONE',  ( 0.000000000000000000, 0.6568589528324747517, -0.7540134720837718962 ) ) ;
#5234 = CARTESIAN_POINT ( 'NONE',  ( 45.81606138205695089, 1.773964314019564448, -3.427682652428129195 ) ) ;
#5235 = VERTEX_POINT ( 'NONE', #6564 ) ;
#5236 = AXIS2_PLACEMENT_3D ( 'NONE', #15476, #11631, #13935 ) ;
#5237 = VERTEX_POINT ( 'NONE', #13924 ) ;
#5238 = VECTOR ( 'NONE', #15143, 1000.000000000000000 ) ;
#5240 = EDGE_CURVE ( 'NONE', #15010, #4631, #10312, .T. ) ;
#5239 = CARTESIAN_POINT ( 'NONE',  ( 46.81606138205697221, -3.676927583119989684, -4.810479898036873259 ) ) ;
#5241 = CARTESIAN_POINT ( 'NONE',  ( 43.06606138205700063, 41.44123852234599070, 73.55501292736987295 ) ) ;
#5242 = EDGE_CURVE ( 'NONE', #23347, #2532, #18302, .T. ) ;
#5243 = CIRCLE ( 'NONE', #8535, 2.500000000000002220 ) ;
#5244 = CARTESIAN_POINT ( 'NONE',  ( 39.02742774030102879, -20.21368208888610241, 72.26730301774234988 ) ) ;
#5245 = VERTEX_POINT ( 'NONE', #19975 ) ;
#5246 = EDGE_CURVE ( 'NONE', #2532, #11164, #18048, .T. ) ;
#5247 = VERTEX_POINT ( 'NONE', #12383 ) ;
#5248 = FACE_OUTER_BOUND ( 'NONE', #17877, .T. ) ;
#5249 = CARTESIAN_POINT ( 'NONE',  ( 38.82593461698262871, 1.086317911113899637, 69.62690120949091011 ) ) ;
#5250 = CARTESIAN_POINT ( 'NONE',  ( 38.26194895904384907, -20.60384086642191548, 73.11602215082116629 ) ) ;
#5251 = CARTESIAN_POINT ( 'NONE',  ( 33.31606138205700773, 7.535758204303438568, 66.26723409915207696 ) ) ;
#5252 = CARTESIAN_POINT ( 'NONE',  ( 36.11133435605973574, -3.613682088886103205, 72.15350918040385864 ) ) ;
#5253 = VERTEX_POINT ( 'NONE', #14299 ) ;
#5254 = VERTEX_POINT ( 'NONE', #20222 ) ;
#5255 = CARTESIAN_POINT ( 'NONE',  ( 40.64099152588522657, 1.142818861812999742, 82.55501292736997243 ) ) ;
#5256 = EDGE_CURVE ( 'NONE', #16707, #9905, #8122, .T. ) ;
#5257 = DIRECTION ( 'NONE',  ( 1.000000000000000000, -0.000000000000000000, 0.000000000000000000 ) ) ;
#5258 = VECTOR ( 'NONE', #5681, 1000.000000000000000 ) ;
#5259 = CARTESIAN_POINT ( 'NONE',  ( 39.59567279493035841, -28.75436684219576833, 70.10737821607207820 ) ) ;
#5260 = AXIS2_PLACEMENT_3D ( 'NONE', #11442, #1386, #22893 ) ;
#5261 = DIRECTION ( 'NONE',  ( 9.027796614315171564E-31, 1.000000000000000000, 1.163336342344340343E-15 ) ) ;
#5262 = DIRECTION ( 'NONE',  ( -1.000000000000000000, -2.999999999999999839E-15, 0.000000000000000000 ) ) ;
#5263 = PLANE ( 'NONE',  #4096 ) ;
#5264 = ORIENTED_EDGE ( 'NONE', *, *, #1421, .F. ) ;
#5265 = CARTESIAN_POINT ( 'NONE',  ( 38.31606138205700063, -11.51539968388051882, 18.41550321377400934 ) ) ;
#5266 = CARTESIAN_POINT ( 'NONE',  ( 38.31606138205700063, -6.959910619544160681, 20.07251914782758107 ) ) ;
#5267 = VERTEX_POINT ( 'NONE', #10066 ) ;
#5268 = ORIENTED_EDGE ( 'NONE', *, *, #8278, .F. ) ;
#5269 = CARTESIAN_POINT ( 'NONE',  ( 36.11133435605973574, -8.003840866421915834, 70.60699637195612866 ) ) ;
#5270 = CARTESIAN_POINT ( 'NONE',  ( 40.31606138205700063, 5.191238522346999673, 69.30501292736998664 ) ) ;
#5271 = CARTESIAN_POINT ( 'NONE',  ( 38.93415946300897446, -18.11368208888611164, 73.09843995877329803 ) ) ;
#5272 = VECTOR ( 'NONE', #4223, 1000.000000000000000 ) ;
#5273 = VECTOR ( 'NONE', #10686, 1000.000000000000114 ) ;
#5274 = VERTEX_POINT ( 'NONE', #22149 ) ;
#5275 = CARTESIAN_POINT ( 'NONE',  ( 33.31606138205697931, -5.022037326221725273, -5.474317061061731771 ) ) ;
#5276 = DIRECTION ( 'NONE',  ( 1.202852874072920494E-15, -0.3934158747763039088, 0.9193606199277819524 ) ) ;
#5277 = CARTESIAN_POINT ( 'NONE',  ( 40.26954217208371034, -22.71368208888610241, 69.89063713639258424 ) ) ;
#5278 = ORIENTED_EDGE ( 'NONE', *, *, #3075, .F. ) ;
#5279 = CARTESIAN_POINT ( 'NONE',  ( 33.80827534892208064, -18.91453975041207158, 24.37026150481227305 ) ) ;
#5280 = CARTESIAN_POINT ( 'NONE',  ( 39.95015449827720744, -2.613682088886105870, 70.79240656858107172 ) ) ;
#5281 = CARTESIAN_POINT ( 'NONE',  ( 29.81606138205707168, -37.26069504592558701, 64.48189387429259511 ) ) ;
#5282 = ADVANCED_FACE ( 'NONE', ( #18175 ), #14048, .T. ) ;
#5283 = CARTESIAN_POINT ( 'NONE',  ( 37.69796330110504101, -15.11368208888609921, 69.66206559358663242 ) ) ;
#5284 = LINE ( 'NONE', #21506, #14344 ) ;
#5285 = FACE_OUTER_BOUND ( 'NONE', #9657, .T. ) ;
#5286 = CARTESIAN_POINT ( 'NONE',  ( 39.37952058850012804, -21.00384086642191050, 71.78268878715390144 ) ) ;
#5287 = CARTESIAN_POINT ( 'NONE',  ( 36.87297107704152666, -5.713682088886105959, 72.49904802271743165 ) ) ;
#5288 = CIRCLE ( 'NONE', #1153, 1.800000000000002931 ) ;
#5289 = ORIENTED_EDGE ( 'NONE', *, *, #23265, .T. ) ;
#5290 = DIRECTION ( 'NONE',  ( -1.836970198721029688E-16, -2.999999999999999839E-15, -1.000000000000000000 ) ) ;
#5291 = ORIENTED_EDGE ( 'NONE', *, *, #10192, .T. ) ;
#5292 = EDGE_LOOP ( 'NONE', ( #15250, #1263, #620, #16960 ) ) ;
#5293 = AXIS2_PLACEMENT_3D ( 'NONE', #11470, #9918, #25083 ) ;
#5294 = CARTESIAN_POINT ( 'NONE',  ( 37.25202387243754032, -2.403840866421914413, 72.75271321436733274 ) ) ;
#5295 = ADVANCED_FACE ( 'NONE', ( #368 ), #497, .T. ) ;
#5296 = AXIS2_PLACEMENT_3D ( 'NONE', #25088, #23431, #25484 ) ;
#5297 = DIRECTION ( 'NONE',  ( 1.000000000000000000, 0.000000000000000000, 0.000000000000000000 ) ) ;
#5298 = EDGE_CURVE ( 'NONE', #19154, #22473, #626, .T. ) ;
#5299 = CARTESIAN_POINT ( 'NONE',  ( 39.82603832034400426, 1.686317911113891732, 72.40698646996136745 ) ) ;
#5300 = ORIENTED_EDGE ( 'NONE', *, *, #16, .F. ) ;
#5301 = CARTESIAN_POINT ( 'NONE',  ( 36.07789103942398867, -7.413682088886105248, 70.70992431699450265 ) ) ;
#5302 = ORIENTED_EDGE ( 'NONE', *, *, #8885, .F. ) ;
#5303 = DIRECTION ( 'NONE',  ( 0.000000000000000000, 2.775557561562888984E-15, 1.000000000000000000 ) ) ;
#5304 = ADVANCED_FACE ( 'NONE', ( #10442 ), #2060, .F. ) ;
#5305 = CARTESIAN_POINT ( 'NONE',  ( 38.63098279924290068, -2.703840866421912015, 72.53360434286905445 ) ) ;
#5306 = AXIS2_PLACEMENT_3D ( 'NONE', #25146, #13581, #23351 ) ;
#5307 = EDGE_CURVE ( 'NONE', #12953, #8151, #6205, .T. ) ;
#5308 = PLANE ( 'NONE',  #13883 ) ;
#5309 = ORIENTED_EDGE ( 'NONE', *, *, #21754, .T. ) ;
#5310 = FACE_OUTER_BOUND ( 'NONE', #21323, .T. ) ;
#5311 = DIRECTION ( 'NONE',  ( 0.000000000000000000, 2.999999999999999839E-15, 1.000000000000000000 ) ) ;
#5312 = CARTESIAN_POINT ( 'NONE',  ( 36.29569395875881099, -18.30384086642191477, 72.77780686321128201 ) ) ;
#5313 = CARTESIAN_POINT ( 'NONE',  ( 36.80559154321147020, -21.53870835236226711, 75.32790188997692837 ) ) ;
#5314 = CIRCLE ( 'NONE', #18061, 2.000000000000001776 ) ;
#5315 = FACE_OUTER_BOUND ( 'NONE', #16277, .T. ) ;
#5316 = CARTESIAN_POINT ( 'NONE',  ( 36.87297107704152666, -17.71368208888610951, 72.49904802271740323 ) ) ;
#5317 = CARTESIAN_POINT ( 'NONE',  ( 36.31606138205700063, 37.94123852234599781, 74.30501292736988717 ) ) ;
#5318 = ADVANCED_FACE ( 'NONE', ( #15966 ), #9938, .T. ) ;
#5319 = CARTESIAN_POINT ( 'NONE',  ( 35.31606138205700773, 7.043113989679085307, 66.83274420321491505 ) ) ;
#5320 = VECTOR ( 'NONE', #19804, 1000.000000000000227 ) ;
#5321 = EDGE_LOOP ( 'NONE', ( #23620, #9382, #22718, #15805, #16767, #22196, #23791, #15435 ) ) ;
#5322 = DIRECTION ( 'NONE',  ( -1.000000000000000000, 6.018531076210110289E-31, 1.734723475976804876E-16 ) ) ;
#5323 = CARTESIAN_POINT ( 'NONE',  ( 36.31606138205700063, -12.87480755223283246, 20.78922580900563588 ) ) ;
#5324 = CARTESIAN_POINT ( 'NONE',  ( 37.25202387243754032, -6.403840866421914413, 72.75271321436733274 ) ) ;
#5325 = ITEM_DEFINED_TRANSFORMATION ( 'NONE', 'NONE', #24436,  #2000 ) ;
#5326 = CARTESIAN_POINT ( 'NONE',  ( 32.81606138205700773, 4.124002793203064066, 6.312068993173404863 ) ) ;
#5327 = VECTOR ( 'NONE', #21485, 1000.000000000000000 ) ;
#5328 = CARTESIAN_POINT ( 'NONE',  ( 40.14115730948191185, -26.51368208888610667, 71.32335560751958781 ) ) ;
#5329 = CARTESIAN_POINT ( 'NONE',  ( 43.31606138205700063, 10.06218483883314718, 67.80501292737497465 ) ) ;
#5330 = CARTESIAN_POINT ( 'NONE',  ( 37.25202387243754032, -24.40384086642191619, 72.75271321436730432 ) ) ;
#5331 = CARTESIAN_POINT ( 'NONE',  ( 36.80507328770344344, -5.887556683877273045, 83.28823336106593445 ) ) ;
#5332 = VECTOR ( 'NONE', #4538, 1000.000000000000000 ) ;
#5333 = CARTESIAN_POINT ( 'NONE',  ( 37.25202387243752611, -21.21368208888610241, 70.00779233799262613 ) ) ;
#5334 = VERTEX_POINT ( 'NONE', #8009 ) ;
#5335 = CARTESIAN_POINT ( 'NONE',  ( 36.07789103942398867, -25.41368208888610525, 70.70992431699450265 ) ) ;
#5336 = ORIENTED_EDGE ( 'NONE', *, *, #20098, .F. ) ;
#5337 = CARTESIAN_POINT ( 'NONE',  ( 32.56606138205700773, -26.74044063519535186, 82.55501292737007191 ) ) ;
#5338 = DIRECTION ( 'NONE',  ( -1.000000000000000000, -1.000000000000000078E-15, 0.000000000000000000 ) ) ;
#5339 = CARTESIAN_POINT ( 'NONE',  ( 38.00113996487114321, -1.913682088886099475, 72.53360434286905445 ) ) ;
#5340 = AXIS2_PLACEMENT_3D ( 'NONE', #18358, #24385, #10505 ) ;
#5341 = EDGE_CURVE ( 'NONE', #5590, #4612, #16069, .T. ) ;
#5342 = VERTEX_POINT ( 'NONE', #23946 ) ;
#5343 = VERTEX_POINT ( 'NONE', #16603 ) ;
#5344 = CARTESIAN_POINT ( 'NONE',  ( 43.81606138205700063, 4.103895195095678794, 6.341006091748962348 ) ) ;
#5345 = DIRECTION ( 'NONE',  ( 0.000000000000000000, 0.3299742535180963943, -0.9439899321577402969 ) ) ;
#5346 = ORIENTED_EDGE ( 'NONE', *, *, #2785, .F. ) ;
#5347 = DIRECTION ( 'NONE',  ( 0.000000000000000000, 0.8191520442889929088, 0.5735764363510444941 ) ) ;
#5348 = CARTESIAN_POINT ( 'NONE',  ( 38.82593461698265003, -2.703840866421916012, 73.13360434286904876 ) ) ;
#5349 = VECTOR ( 'NONE', #6650, 1000.000000000000000 ) ;
#5350 = DIRECTION ( 'NONE',  ( 9.925461516413211857E-16, -0.8967398287344598984, -0.4425581086832454658 ) ) ;
#5351 = LINE ( 'NONE', #14626, #24140 ) ;
#5352 = ORIENTED_EDGE ( 'NONE', *, *, #6293, .T. ) ;
#5353 = AXIS2_PLACEMENT_3D ( 'NONE', #17531, #19577, #6056 ) ;
#5354 = CARTESIAN_POINT ( 'NONE',  ( 35.31606138205700773, 3.296535697557906985, 65.33616386252352015 ) ) ;
#5355 = CARTESIAN_POINT ( 'NONE',  ( 38.82593461698262871, 1.086317911113899637, 69.62690120949092432 ) ) ;
#5356 = ORIENTED_EDGE ( 'NONE', *, *, #23410, .T. ) ;
#5357 = CARTESIAN_POINT ( 'NONE',  ( 36.87297107704151244, -25.90384086642190908, 70.26145752964252722 ) ) ;
#5358 = CARTESIAN_POINT ( 'NONE',  ( 43.30090830489194786, -32.87633672316712108, 59.29685926994373091 ) ) ;
#5359 = CIRCLE ( 'NONE', #7767, 1.000000000000000888 ) ;
#5360 = ORIENTED_EDGE ( 'NONE', *, *, #18074, .F. ) ;
#5361 = VECTOR ( 'NONE', #12412, 1000.000000000000227 ) ;
#5362 = DIRECTION ( 'NONE',  ( 1.000000000000000000, 0.000000000000000000, 0.000000000000000000 ) ) ;
#5363 = EDGE_CURVE ( 'NONE', #22433, #8848, #18671, .T. ) ;
#5364 = VECTOR ( 'NONE', #8564, 1000.000000000000000 ) ;
#5365 = CARTESIAN_POINT ( 'NONE',  ( 31.56606138205697576, -5.022037326221730602, -5.474317061061731771 ) ) ;
#5366 = DIRECTION ( 'NONE',  ( 1.000000000000000000, 0.000000000000000000, 0.000000000000000000 ) ) ;
#5367 = VERTEX_POINT ( 'NONE', #16868 ) ;
#5368 = DIRECTION ( 'NONE',  ( 0.000000000000000000, -1.000000000000000000, 2.999999999999999839E-15 ) ) ;
#5369 = EDGE_LOOP ( 'NONE', ( #5055, #12894, #7801, #16896, #7175, #25019, #6610, #5586, #22075, #7490, #4164, #1547, #3299, #13979, #20269, #15713, #6161, #7815, #3020 ) ) ;
#5370 = VERTEX_POINT ( 'NONE', #4885 ) ;
#5371 = LINE ( 'NONE', #14770, #6267 ) ;
#5372 = CARTESIAN_POINT ( 'NONE',  ( 44.81606138205700063, -36.55876147765400930, 73.30501292737011454 ) ) ;
#5373 = CARTESIAN_POINT ( 'NONE',  ( 37.38336156205274818, -17.71368208888609885, 72.12822762946750288 ) ) ;
#5374 = ORIENTED_EDGE ( 'NONE', *, *, #14624, .T. ) ;
#5375 = ORIENTED_EDGE ( 'NONE', *, *, #729, .F. ) ;
#5376 = DIRECTION ( 'NONE',  ( -0.000000000000000000, -3.469446951953613400E-15, -1.000000000000000000 ) ) ;
#5377 = CARTESIAN_POINT ( 'NONE',  ( 31.56606138205697576, -5.918777154956194053, -5.916875169744970187 ) ) ;
#5378 = CARTESIAN_POINT ( 'NONE',  ( 38.37017380507018771, -23.60384086642190837, 69.64448340153877837 ) ) ;
#5379 = LINE ( 'NONE', #17108, #12458 ) ;
#5380 = AXIS2_PLACEMENT_3D ( 'NONE', #1004, #6816, #20468 ) ;
#5381 = ORIENTED_EDGE ( 'NONE', *, *, #10858, .F. ) ;
#5382 = DIRECTION ( 'NONE',  ( 1.000000000000000000, -0.000000000000000000, -0.000000000000000000 ) ) ;
#5383 = CARTESIAN_POINT ( 'NONE',  ( 46.81606138205695800, -0.2703287878657641974, 1.505452687840413972 ) ) ;
#5384 = ADVANCED_FACE ( 'NONE', ( #10701 ), #20607, .T. ) ;
#5385 = LINE ( 'NONE', #1498, #2142 ) ;
#5386 = ADVANCED_FACE ( 'NONE', ( #12632 ), #3198, .T. ) ;
#5387 = CARTESIAN_POINT ( 'NONE',  ( 38.31606138205700063, -5.204193249396277032, 83.30501292736992980 ) ) ;
#5388 = DIRECTION ( 'NONE',  ( -0.000000000000000000, -0.9814242980364923374, -0.1918498038142812112 ) ) ;
#5389 = EDGE_CURVE ( 'NONE', #10647, #11848, #9021, .T. ) ;
#5390 = B_SPLINE_SURFACE_WITH_KNOTS ( 'NONE', 1, 3, ( 
 ( #23018, #15542, #19409, #7314 ),
 ( #11575, #9267, #13381, #3447 ) ),
 .UNSPECIFIED., .F., .F., .F.,
 ( 2, 2 ),
 ( 4, 4 ),
 ( 0.000000000000000000, 1.000000000000000000 ),
 ( 0.000000000000000000, 1.000000000000000000 ),
 .UNSPECIFIED. ) ;
#5391 = CARTESIAN_POINT ( 'NONE',  ( 44.81606138205700063, 0.1601050959395486362, 68.80395113470939350 ) ) ;
#5392 = VERTEX_POINT ( 'NONE', #4757 ) ;
#5393 = CARTESIAN_POINT ( 'NONE',  ( 36.81606138205700063, -7.415330352220093069, 56.88974067930232081 ) ) ;
#5394 = DIRECTION ( 'NONE',  ( -1.000000000000000000, 0.000000000000000000, 0.000000000000000000 ) ) ;
#5395 = ORIENTED_EDGE ( 'NONE', *, *, #15441, .F. ) ;
#5396 = ORIENTED_EDGE ( 'NONE', *, *, #7696, .T. ) ;
#5397 = UNCERTAINTY_MEASURE_WITH_UNIT (LENGTH_MEASURE( 1.000000000000000082E-05 ), #23294, 'distance_accuracy_value', 'NONE');
#5398 = VECTOR ( 'NONE', #19032, 1000.000000000000000 ) ;
#5399 = CARTESIAN_POINT ( 'NONE',  ( 36.07789103942399578, -12.20384086642191512, 72.05058123536544201 ) ) ;
#5400 = EDGE_CURVE ( 'NONE', #25120, #22481, #24564, .T. ) ;
#5401 = DIRECTION ( 'NONE',  ( 1.734723475976805122E-16, -1.000000000000000000, 0.000000000000000000 ) ) ;
#5402 = CARTESIAN_POINT ( 'NONE',  ( 36.64852494920107517, -13.41368208888610525, 70.89533451361947414 ) ) ;
#5403 =( NAMED_UNIT ( * ) PLANE_ANGLE_UNIT ( ) SI_UNIT ( $, .RADIAN. ) );
#5404 = ORIENTED_EDGE ( 'NONE', *, *, #14904, .F. ) ;
#5405 = LINE ( 'NONE', #25473, #18747 ) ;
#5406 = LINE ( 'NONE', #7599, #8403 ) ;
#5407 = CARTESIAN_POINT ( 'NONE',  ( 39.73277004305198545, -18.21368208888610596, 73.23812341099225875 ) ) ;
#5408 = ORIENTED_EDGE ( 'NONE', *, *, #7068, .F. ) ;
#5409 = FACE_BOUND ( 'NONE', #10337, .T. ) ;
#5410 = CARTESIAN_POINT ( 'NONE',  ( 47.81606138205697931, -4.589472609077211551, -6.350807634294790560 ) ) ;
#5411 = DIRECTION ( 'NONE',  ( 1.734723475976804876E-16, -1.163336342344340343E-15, 1.000000000000000000 ) ) ;
#5412 = AXIS2_PLACEMENT_3D ( 'NONE', #4339, #12201, #20040 ) ;
#5413 = LINE ( 'NONE', #5543, #7357 ) ;
#5414 = CIRCLE ( 'NONE', #887, 1.500000000000006217 ) ;
#5415 = CARTESIAN_POINT ( 'NONE',  ( 32.56606138205700773, 40.39281886181299797, 83.30501292736984453 ) ) ;
#5416 = CARTESIAN_POINT ( 'NONE',  ( 38.37017380507018771, -15.60384086642191370, 70.24448340153875847 ) ) ;
#5417 = CARTESIAN_POINT ( 'NONE',  ( 37.25202387243752611, 0.7863179111138978161, 70.00779233799264034 ) ) ;
#5418 = EDGE_LOOP ( 'NONE', ( #7672, #23825, #21806, #9250 ) ) ;
#5419 = CARTESIAN_POINT ( 'NONE',  ( 32.81606138205700773, -38.55876147765400219, 75.30501292737012875 ) ) ;
#5420 = CARTESIAN_POINT ( 'NONE',  ( 36.81606138205700063, -1.383222575549920119, 62.14461230196212682 ) ) ;
#5421 = ORIENTED_EDGE ( 'NONE', *, *, #16024, .T. ) ;
#5422 = ORIENTED_EDGE ( 'NONE', *, *, #23086, .F. ) ;
#5423 = CARTESIAN_POINT ( 'NONE',  ( 40.14115730948191185, 0.8961591335780898504, 71.43714994484035685 ) ) ;
#5424 = EDGE_CURVE ( 'NONE', #13993, #1915, #14022, .T. ) ;
#5425 = CARTESIAN_POINT ( 'NONE',  ( 38.37017380507020192, -28.01368208888610312, 72.51602215082114355 ) ) ;
#5426 = CARTESIAN_POINT ( 'NONE',  ( 40.77203464402485622, -4.513682088886104893, 71.32335560751961623 ) ) ;
#5427 = ORIENTED_EDGE ( 'NONE', *, *, #3113, .T. ) ;
#5428 = CARTESIAN_POINT ( 'NONE',  ( 38.31606138205700063, -6.959910619544160681, 20.07251914782758107 ) ) ;
#5429 = VECTOR ( 'NONE', #23922, 1000.000000000000000 ) ;
#5430 = CARTESIAN_POINT ( 'NONE',  ( 37.31647492878124694, -6.303840866421912104, 72.03616607671141026 ) ) ;
#5431 = CYLINDRICAL_SURFACE ( 'NONE', #24550, 3.000000000000002665 ) ;
#5432 = ORIENTED_EDGE ( 'NONE', *, *, #6671, .F. ) ;
#5433 = CARTESIAN_POINT ( 'NONE',  ( 34.06606138205700773, -37.81581049437288300, 70.47722359350072452 ) ) ;
#5434 = PLANE ( 'NONE',  #1776 ) ;
#5435 = VECTOR ( 'NONE', #6960, 1000.000000000000000 ) ;
#5436 = CARTESIAN_POINT ( 'NONE',  ( 36.11133435605973574, -8.003840866421915834, 70.60699637195612866 ) ) ;
#5437 = CARTESIAN_POINT ( 'NONE',  ( 37.79585267494195477, -22.15694282365413059, 75.30518664689680008 ) ) ;
#5438 = CARTESIAN_POINT ( 'NONE',  ( 37.14448850680319225, -21.82678658219788304, 29.70634659473178374 ) ) ;
#5439 = CARTESIAN_POINT ( 'NONE',  ( 39.38009889167650357, -16.21368208888610596, 72.75271321436731853 ) ) ;
#5440 = DIRECTION ( 'NONE',  ( 0.000000000000000000, -6.938893903907222067E-15, 1.000000000000000000 ) ) ;
#5441 = LINE ( 'NONE', #1556, #18388 ) ;
#5442 = VERTEX_POINT ( 'NONE', #20474 ) ;
#5443 = CARTESIAN_POINT ( 'NONE',  ( 43.81606138205700063, 41.44123852234595518, 61.30501292736988006 ) ) ;
#5444 = CARTESIAN_POINT ( 'NONE',  ( 39.95015449827720744, -9.003840866421912281, 71.96809898377888715 ) ) ;
#5445 = APPLICATION_PROTOCOL_DEFINITION ( 'draft international standard', 'automotive_design', 1998, #6029 ) ;
#5446 = VECTOR ( 'NONE', #2139, 1000.000000000000000 ) ;
#5447 = CARTESIAN_POINT ( 'NONE',  ( 32.81606138205700773, 2.740850673309605412, 6.112030963703427133 ) ) ;
#5448 = CARTESIAN_POINT ( 'NONE',  ( 36.80608444377001121, -17.31368208888609672, 70.35351908239857721 ) ) ;
#5449 = DIRECTION ( 'NONE',  ( -1.000000000000000000, 0.000000000000000000, 0.000000000000000000 ) ) ;
#5450 = VECTOR ( 'NONE', #4338, 1000.000000000000000 ) ;
#5451 = CARTESIAN_POINT ( 'NONE',  ( 39.82603832034400426, -17.30384086642190056, 70.35351908239857721 ) ) ;
#5452 = CARTESIAN_POINT ( 'NONE',  ( 38.05217264712879199, -5.216727773490275943, 82.80503503306502466 ) ) ;
#5453 = VECTOR ( 'NONE', #22391, 1000.000000000000000 ) ;
#5454 = CARTESIAN_POINT ( 'NONE',  ( 36.64852494920107517, -17.41368208888610525, 70.89533451361947414 ) ) ;
#5455 = EDGE_LOOP ( 'NONE', ( #3930, #20016, #2657, #16724 ) ) ;
#5456 = CARTESIAN_POINT ( 'NONE',  ( 40.26954217208371034, -28.71368208888610241, 69.89063713639254161 ) ) ;
#5457 = VECTOR ( 'NONE', #24680, 1000.000000000000000 ) ;
#5458 = ORIENTED_EDGE ( 'NONE', *, *, #21854, .T. ) ;
#5459 = DIRECTION ( 'NONE',  ( -1.000000000000000000, 0.000000000000000000, 0.000000000000000000 ) ) ;
#5460 = FACE_OUTER_BOUND ( 'NONE', #3367, .T. ) ;
#5461 = CARTESIAN_POINT ( 'NONE',  ( 39.51027997493896748, -23.10384086642191548, 71.43714994484032843 ) ) ;
#5462 = ORIENTED_EDGE ( 'NONE', *, *, #12289, .T. ) ;
#5463 = ORIENTED_EDGE ( 'NONE', *, *, #25288, .F. ) ;
#5464 = DIRECTION ( 'NONE',  ( 0.000000000000000000, 0.6568589528324747517, -0.7540134720837717852 ) ) ;
#5465 = DIRECTION ( 'NONE',  ( -1.000000000000000078E-15, 0.9439899321577400748, 0.3299742535180970049 ) ) ;
#5466 = ORIENTED_EDGE ( 'NONE', *, *, #21629, .T. ) ;
#5467 = CARTESIAN_POINT ( 'NONE',  ( 31.81606138205700418, 35.44123852234597649, 67.80501292736990138 ) ) ;
#5468 = CARTESIAN_POINT ( 'NONE',  ( 37.50301148336529877, -28.50384086642192116, 73.69843995877326392 ) ) ;
#5469 = VECTOR ( 'NONE', #11545, 1000.000000000000000 ) ;
#5470 = PLANE ( 'NONE',  #13757 ) ;
#5471 = AXIS2_PLACEMENT_3D ( 'NONE', #8163, #6100, #12170 ) ;
#5472 = DIRECTION ( 'NONE',  ( -3.965082230804126670E-15, 1.000000000000000000, 0.000000000000000000 ) ) ;
#5473 = ORIENTED_EDGE ( 'NONE', *, *, #17933, .T. ) ;
#5474 = EDGE_CURVE ( 'NONE', #1520, #5143, #23469, .T. ) ;
#5475 = ORIENTED_EDGE ( 'NONE', *, *, #2155, .F. ) ;
#5476 = DIRECTION ( 'NONE',  ( 0.000000000000000000, 1.000000000000000000, -4.625929269271481378E-15 ) ) ;
#5477 = ADVANCED_FACE ( 'NONE', ( #14667 ), #20738, .F. ) ;
#5478 = CARTESIAN_POINT ( 'NONE',  ( 32.81606138205700773, 16.19123852234701388, 73.80501292736995822 ) ) ;
#5479 = VECTOR ( 'NONE', #18003, 1000.000000000000000 ) ;
#5480 = CARTESIAN_POINT ( 'NONE',  ( 39.38009889167648936, -27.40384086642190908, 70.00779233799262613 ) ) ;
#5481 = EDGE_CURVE ( 'NONE', #19237, #8412, #20, .T. ) ;
#5482 = FILL_AREA_STYLE ('',( #19256 ) ) ;
#5483 = CARTESIAN_POINT ( 'NONE',  ( 43.31606138205700063, -33.36512800456291217, 60.17493404035838012 ) ) ;
#5484 = EDGE_CURVE ( 'NONE', #8869, #5253, #3072, .T. ) ;
#5485 = EDGE_CURVE ( 'NONE', #6235, #15007, #12886, .T. ) ;
#5486 = ORIENTED_EDGE ( 'NONE', *, *, #3089, .F. ) ;
#5487 = DIRECTION ( 'NONE',  ( -5.421010862427517856E-17, 0.7540134720837717852, 0.6568589528324746407 ) ) ;
#5488 = VECTOR ( 'NONE', #5577, 1000.000000000000000 ) ;
#5489 = CARTESIAN_POINT ( 'NONE',  ( 43.81606138205700063, 35.95440708241085304, 62.30501292736990138 ) ) ;
#5490 = FACE_OUTER_BOUND ( 'NONE', #4456, .T. ) ;
#5491 = FILL_AREA_STYLE ('',( #1234 ) ) ;
#5492 = ORIENTED_EDGE ( 'NONE', *, *, #477, .F. ) ;
#5493 = AXIS2_PLACEMENT_3D ( 'NONE', #16908, #11248, #24604 ) ;
#5494 = ADVANCED_FACE ( 'NONE', ( #6687 ), #10945, .F. ) ;
#5495 = FACE_OUTER_BOUND ( 'NONE', #7713, .T. ) ;
#5496 = EDGE_LOOP ( 'NONE', ( #2029, #8955, #17096, #22123 ) ) ;
#5497 = VERTEX_POINT ( 'NONE', #13009 ) ;
#5498 = EDGE_CURVE ( 'NONE', #14863, #6167, #24316, .T. ) ;
#5499 = DIRECTION ( 'NONE',  ( 0.000000000000000000, -0.7540134720837717852, -0.6568589528324746407 ) ) ;
#5500 = CARTESIAN_POINT ( 'NONE',  ( 37.12184278917507640, -9.513682088886101340, 71.43714994484035685 ) ) ;
#5501 = CARTESIAN_POINT ( 'NONE',  ( 38.26194895904383486, -11.01368208888609956, 70.24448340153877268 ) ) ;
#5502 = ORIENTED_EDGE ( 'NONE', *, *, #12367, .T. ) ;
#5503 = CIRCLE ( 'NONE', #8390, 3.999999999999996447 ) ;
#5504 = EDGE_LOOP ( 'NONE', ( #7618, #9747, #20329, #5152 ) ) ;
#5505 = CARTESIAN_POINT ( 'NONE',  ( 36.31606138205700063, 37.94123852234599070, 73.55501292736988717 ) ) ;
#5506 = DIRECTION ( 'NONE',  ( 3.965082230804125881E-15, -0.8967398287344645613, -0.4425581086832361399 ) ) ;
#5507 = CARTESIAN_POINT ( 'NONE',  ( 40.14115730948191185, -21.10384086642191193, 71.43714994484030001 ) ) ;
#5508 = STYLED_ITEM ( 'NONE', ( #2940 ), #8595 ) ;
#5509 = CARTESIAN_POINT ( 'NONE',  ( 42.56606138205700063, 2.736744647373098971, 6.109177798617293931 ) ) ;
#5510 = EDGE_CURVE ( 'NONE', #9479, #9779, #17000, .T. ) ;
#5511 = CARTESIAN_POINT ( 'NONE',  ( 37.21915885897815457, -21.41368208888610525, 71.08074471024443142 ) ) ;
#5512 = ORIENTED_EDGE ( 'NONE', *, *, #11569, .F. ) ;
#5513 = VECTOR ( 'NONE', #3724, 1000.000000000000000 ) ;
#5514 = ORIENTED_EDGE ( 'NONE', *, *, #14200, .F. ) ;
#5515 = DIRECTION ( 'NONE',  ( 6.109829820097539848E-16, -0.6595716529892418079, 0.7516416929448760387 ) ) ;
#5516 = VECTOR ( 'NONE', #15565, 1000.000000000000227 ) ;
#5517 = DIRECTION ( 'NONE',  ( -1.000000000000000000, -3.046270958365671426E-15, 5.272995181423179347E-17 ) ) ;
#5518 = DIRECTION ( 'NONE',  ( 0.000000000000000000, 2.999999999999999839E-15, 1.000000000000000000 ) ) ;
#5519 = CARTESIAN_POINT ( 'NONE',  ( 38.31606138205700063, -5.204193249396280585, 82.80501292736992980 ) ) ;
#5520 = LINE ( 'NONE', #3697, #15964 ) ;
#5521 = DIRECTION ( 'NONE',  ( 3.540251991789399939E-16, 2.999999999999999839E-15, 1.000000000000000000 ) ) ;
#5522 = VERTEX_POINT ( 'NONE', #23260 ) ;
#5523 = COLOUR_RGB ( '', 0.08235294, 0.09019608, 0.10196078) ;
#5524 = CARTESIAN_POINT ( 'NONE',  ( 33.56606138205700773, 41.44123852234599070, 73.55501292736987295 ) ) ;
#5525 = DIRECTION ( 'NONE',  ( 0.000000000000000000, -2.999999999999999839E-15, -1.000000000000000000 ) ) ;
#5526 = ORIENTED_EDGE ( 'NONE', *, *, #19837, .F. ) ;
#5527 = EDGE_LOOP ( 'NONE', ( #16003, #13218 ) ) ;
#5528 = AXIS2_PLACEMENT_3D ( 'NONE', #10511, #18365, #2748 ) ;
#5529 = AXIS2_PLACEMENT_3D ( 'NONE', #10249, #4705, #12317 ) ;
#5530 = CARTESIAN_POINT ( 'NONE',  ( 39.64521430340305841, -10.80384086642191832, 73.30173637941818754 ) ) ;
#5531 = VECTOR ( 'NONE', #6893, 1000.000000000000114 ) ;
#5532 = CARTESIAN_POINT ( 'NONE',  ( 33.81606138205700063, 2.191238522347013440, 73.80501292737000085 ) ) ;
#5533 = CARTESIAN_POINT ( 'NONE',  ( 36.87297107704152666, -17.71368208888610951, 72.49904802271740323 ) ) ;
#5534 = ORIENTED_EDGE ( 'NONE', *, *, #18690, .F. ) ;
#5535 = FACE_OUTER_BOUND ( 'NONE', #20099, .T. ) ;
#5536 = CARTESIAN_POINT ( 'NONE',  ( 32.81606138205700773, -37.98241563432386414, 69.85268917996594951 ) ) ;
#5537 = CARTESIAN_POINT ( 'NONE',  ( 36.36258059203031934, -21.71368208888610596, 72.86986841596736042 ) ) ;
#5538 = ORIENTED_EDGE ( 'NONE', *, *, #5389, .T. ) ;
#5539 = CARTESIAN_POINT ( 'NONE',  ( 35.56606138205698642, -9.092667827980710271, 28.75914562266559926 ) ) ;
#5540 = PRODUCT_DEFINITION_FORMATION_WITH_SPECIFIED_SOURCE ( 'ANY', '', #19167, .NOT_KNOWN. ) ;
#5541 = CARTESIAN_POINT ( 'NONE',  ( 32.81606138205700773, 46.92314894770294131, 81.17823623207318917 ) ) ;
#5542 = DIRECTION ( 'NONE',  ( 4.336808689942074435E-17, -1.000000000000000000, 3.491481338843135327E-15 ) ) ;
#5543 = CARTESIAN_POINT ( 'NONE',  ( 35.81606138205700063, -24.05876147765399864, 75.30501292737008612 ) ) ;
#5544 = CARTESIAN_POINT ( 'NONE',  ( 37.42710149357921523, -5.407787168292675695, 83.30316041875967414 ) ) ;
#5545 = CARTESIAN_POINT ( 'NONE',  ( 39.24876120206129571, -10.90384086642191264, 72.12822762946750288 ) ) ;
#5546 = CARTESIAN_POINT ( 'NONE',  ( 37.33957961208646736, 0.1863179111138910105, 72.81632618279323310 ) ) ;
#5547 = ORIENTED_EDGE ( 'NONE', *, *, #22637, .T. ) ;
#5548 = DIRECTION ( 'NONE',  ( 0.000000000000000000, -1.000000000000000000, 2.999999999999999839E-15 ) ) ;
#5549 = LINE ( 'NONE', #9426, #13990 ) ;
#5550 = ORIENTED_EDGE ( 'NONE', *, *, #12112, .F. ) ;
#5551 = ORIENTED_EDGE ( 'NONE', *, *, #24334, .F. ) ;
#5552 = CARTESIAN_POINT ( 'NONE',  ( 39.29254315202757653, 1.196159133578084788, 72.81632618279324731 ) ) ;
#5553 = CARTESIAN_POINT ( 'NONE',  ( 37.25202387243752611, 0.7863179111138978161, 70.00779233799264034 ) ) ;
#5554 = CARTESIAN_POINT ( 'NONE',  ( 36.98690846071097837, -3.813682088886109156, 73.30173637941818754 ) ) ;
#5555 = VERTEX_POINT ( 'NONE', #12516 ) ;
#5556 = CARTESIAN_POINT ( 'NONE',  ( 31.91606138205697363, -3.854803714928949798, -5.706129749257958572 ) ) ;
#5557 = VECTOR ( 'NONE', #21244, 1000.000000000000000 ) ;
#5558 = ADVANCED_FACE ( 'NONE', ( #20354 ), #2683, .T. ) ;
#5559 = CARTESIAN_POINT ( 'NONE',  ( 37.21915885897815457, -4.203840866421909794, 71.67976084211552745 ) ) ;
#5560 = ADVANCED_FACE ( 'NONE', ( #16470 ), #19533, .T. ) ;
#5561 = LINE ( 'NONE', #9437, #8963 ) ;
#5562 = ORIENTED_EDGE ( 'NONE', *, *, #20361, .T. ) ;
#5563 = CARTESIAN_POINT ( 'NONE',  ( 30.81606138205700418, -36.05876147765410877, 70.30501292737000085 ) ) ;
#5564 = PLANE ( 'NONE',  #11684 ) ;
#5565 = CARTESIAN_POINT ( 'NONE',  ( 36.36258059203030513, -9.903840866421909084, 69.89063713639259845 ) ) ;
#5566 = CARTESIAN_POINT ( 'NONE',  ( 32.81606138205700773, -1.963190818658398173, 19.89143565483009013 ) ) ;
#5567 = CARTESIAN_POINT ( 'NONE',  ( 43.81606138205700063, 44.92314894770294131, 81.17823623207320338 ) ) ;
#5568 = CARTESIAN_POINT ( 'NONE',  ( 37.69796330110504101, -13.11368208888609743, 69.66206559358661821 ) ) ;
#5569 = CARTESIAN_POINT ( 'NONE',  ( 43.31606138205700063, 9.733755362416909307, 68.18201966341686671 ) ) ;
#5570 = CARTESIAN_POINT ( 'NONE',  ( 43.23147868389327897, 40.76768529863396395, 79.57823623207325170 ) ) ;
#5571 = ORIENTED_EDGE ( 'NONE', *, *, #13684, .F. ) ;
#5572 = PLANE ( 'NONE',  #8965 ) ;
#5573 = ADVANCED_FACE ( 'NONE', ( #15662 ), #17739, .T. ) ;
#5574 = CARTESIAN_POINT ( 'NONE',  ( 39.38009889167648936, -5.403840866421906419, 70.00779233799264034 ) ) ;
#5575 = VECTOR ( 'NONE', #6692, 1000.000000000000000 ) ;
#5576 = SHAPE_DEFINITION_REPRESENTATION ( #25327, #9445 ) ;
#5577 = DIRECTION ( 'NONE',  ( 1.000000000000000000, 1.734723475976804876E-16, -1.734723475976814737E-16 ) ) ;
#5578 = AXIS2_PLACEMENT_3D ( 'NONE', #24330, #8264, #6334 ) ;
#5579 = CARTESIAN_POINT ( 'NONE',  ( 36.64852494920107517, -15.41368208888610525, 70.89533451361947414 ) ) ;
#5580 = CARTESIAN_POINT ( 'NONE',  ( 38.31606138205700063, -3.742417511052531509, 58.76316301854844681 ) ) ;
#5581 = CARTESIAN_POINT ( 'NONE',  ( 36.68196826583682935, -16.00384086642191050, 70.79240656858107172 ) ) ;
#5582 = CYLINDRICAL_SURFACE ( 'NONE', #4807, 0.7500000000000027756 ) ;
#5583 = CARTESIAN_POINT ( 'NONE',  ( 36.49096545463212493, -15.51368208888610667, 71.43714994484034264 ) ) ;
#5584 = ORIENTED_EDGE ( 'NONE', *, *, #15612, .F. ) ;
#5585 = CARTESIAN_POINT ( 'NONE',  ( 36.07789103942398867, -21.41368208888610880, 70.70992431699450265 ) ) ;
#5586 = ORIENTED_EDGE ( 'NONE', *, *, #10169, .F. ) ;
#5587 = DIRECTION ( 'NONE',  ( -1.734723475976807292E-15, 0.7516416929448820339, 0.6595716529892350355 ) ) ;
#5588 = DIRECTION ( 'NONE',  ( -2.048868001712896742E-15, 0.6595716529892345914, -0.7516416929448823669 ) ) ;
#5589 = CARTESIAN_POINT ( 'NONE',  ( 39.51027997493896748, -27.10384086642191903, 71.43714994484031422 ) ) ;
#5590 = VERTEX_POINT ( 'NONE', #5880 ) ;
#5591 = ORIENTED_EDGE ( 'NONE', *, *, #3899, .F. ) ;
#5592 = FACE_OUTER_BOUND ( 'NONE', #15594, .T. ) ;
#5593 = DIRECTION ( 'NONE',  ( 1.000000000000000000, 2.999999999999999839E-15, 0.000000000000000000 ) ) ;
#5594 = ORIENTED_EDGE ( 'NONE', *, *, #12133, .F. ) ;
#5595 = CARTESIAN_POINT ( 'NONE',  ( 39.82603832034400426, 0.6961591335780910050, 70.35351908239860563 ) ) ;
#5596 = CARTESIAN_POINT ( 'NONE',  ( 38.31606138205700063, -29.30876147765400930, 71.30501292737010033 ) ) ;
#5597 = PRODUCT_DEFINITION_SHAPE ( 'NONE', 'NONE',  #23001 ) ;
#5598 = CARTESIAN_POINT ( 'NONE',  ( 33.31606138205700773, 7.043113989679085307, 66.83274420321491505 ) ) ;
#5599 = EDGE_LOOP ( 'NONE', ( #1485, #22225, #16839, #23920 ) ) ;
#5600 = EDGE_LOOP ( 'NONE', ( #6712, #11975 ) ) ;
#5601 = FACE_OUTER_BOUND ( 'NONE', #16538, .T. ) ;
#5602 = CARTESIAN_POINT ( 'NONE',  ( 44.81606138205700063, 41.44123852234599070, 73.55501292736987295 ) ) ;
#5603 = EDGE_CURVE ( 'NONE', #10371, #11274, #16904, .T. ) ;
#5604 = CARTESIAN_POINT ( 'NONE',  ( 40.14115730948191185, -27.10384086642191193, 71.43714994484030001 ) ) ;
#5605 = DIRECTION ( 'NONE',  ( 1.000000000000000000, 0.000000000000000000, 0.000000000000000000 ) ) ;
#5606 = LINE ( 'NONE', #21319, #4869 ) ;
#5607 = DIRECTION ( 'NONE',  ( -4.336808689942020201E-16, -2.999999999999999839E-15, -1.000000000000000000 ) ) ;
#5608 = LINE ( 'NONE', #3794, #9351 ) ;
#5609 = CARTESIAN_POINT ( 'NONE',  ( 39.37952058850012804, -5.003840866421912281, 71.78268878715392987 ) ) ;
#5610 = ORIENTED_EDGE ( 'NONE', *, *, #15972, .T. ) ;
#5611 = CARTESIAN_POINT ( 'NONE',  ( 30.81606138205700418, 40.39281886181299797, 82.55501292736983032 ) ) ;
#5612 = ORIENTED_EDGE ( 'NONE', *, *, #14434, .F. ) ;
#5613 = EDGE_LOOP ( 'NONE', ( #19666, #7306, #10537, #23116 ) ) ;
#5614 = CARTESIAN_POINT ( 'NONE',  ( 44.81606138205700063, 1.441238522345976714, 67.80501292737001506 ) ) ;
#5615 = CARTESIAN_POINT ( 'NONE',  ( 38.00113996487114321, -13.91368208888610347, 72.53360434286904024 ) ) ;
#5616 = EDGE_CURVE ( 'NONE', #13887, #14165, #23652, .T. ) ;
#5617 = EDGE_CURVE ( 'NONE', #9497, #4779, #2082, .T. ) ;
#5618 = CARTESIAN_POINT ( 'NONE',  ( 39.31564783533280405, -10.31368208888610027, 72.03616607671141026 ) ) ;
#5619 = ORIENTED_EDGE ( 'NONE', *, *, #10532, .F. ) ;
#5620 = ORIENTED_EDGE ( 'NONE', *, *, #11152, .T. ) ;
#5621 = DIRECTION ( 'NONE',  ( 1.000000000000000000, -6.938893903907222067E-15, 0.000000000000000000 ) ) ;
#5622 = DIRECTION ( 'NONE',  ( -1.000000000000000000, -3.469446951953611033E-15, 0.000000000000000000 ) ) ;
#5623 = EDGE_LOOP ( 'NONE', ( #15814, #4131, #21557, #25354 ) ) ;
#5624 = FACE_OUTER_BOUND ( 'NONE', #7098, .T. ) ;
#5625 = CARTESIAN_POINT ( 'NONE',  ( 36.80608444377001831, -14.30384086642191122, 72.40698646996135324 ) ) ;
#5626 = EDGE_CURVE ( 'NONE', #18958, #11492, #9510, .T. ) ;
#5627 = EDGE_CURVE ( 'NONE', #6274, #24574, #17868, .T. ) ;
#5628 = CARTESIAN_POINT ( 'NONE',  ( 42.99945007810772069, 2.836788837719289802, 6.100487119615180198 ) ) ;
#5629 = CARTESIAN_POINT ( 'NONE',  ( 38.93987200065208754, -18.81368208888610027, 70.42958956619168021 ) ) ;
#5630 = ORIENTED_EDGE ( 'NONE', *, *, #9002, .T. ) ;
#5631 = FACE_OUTER_BOUND ( 'NONE', #13241, .T. ) ;
#5632 = ADVANCED_FACE ( 'NONE', ( #2123 ), #23382, .F. ) ;
#5633 = LINE ( 'NONE', #17360, #8555 ) ;
#5634 = CARTESIAN_POINT ( 'NONE',  ( 31.81606138205700418, -24.55876147765401285, 70.30501292737008612 ) ) ;
#5635 = CARTESIAN_POINT ( 'NONE',  ( 39.32110845963273960, -5.457363569681777271, 82.80205412878008531 ) ) ;
#5636 = CARTESIAN_POINT ( 'NONE',  ( 38.31606138205700063, -6.959910619544160681, 20.07251914782758107 ) ) ;
#5637 = AXIS2_PLACEMENT_3D ( 'NONE', #4467, #6268, #8459 ) ;
#5638 = DIRECTION ( 'NONE',  ( -1.000000000000000275E-15, 0.9439899321577401858, 0.3299742535180970604 ) ) ;
#5639 = CIRCLE ( 'NONE', #6869, 1.500000000000001332 ) ;
#5640 = VERTEX_POINT ( 'NONE', #6009 ) ;
#5641 = CARTESIAN_POINT ( 'NONE',  ( 43.39391466435952793, 3.105264735555241629, 6.136852473770347594 ) ) ;
#5642 = VERTEX_POINT ( 'NONE', #316 ) ;
#5643 = ORIENTED_EDGE ( 'NONE', *, *, #7858, .F. ) ;
#5644 = CARTESIAN_POINT ( 'NONE',  ( 36.29569395875881099, -10.30384086642191832, 72.77780686321129622 ) ) ;
#5645 = CARTESIAN_POINT ( 'NONE',  ( 38.31606138205700063, -7.086900875803856970, 56.51273394326043586 ) ) ;
#5646 = CARTESIAN_POINT ( 'NONE',  ( 39.38009889167650357, -16.21368208888610596, 72.75271321436731853 ) ) ;
#5647 = EDGE_CURVE ( 'NONE', #17700, #4468, #12071, .T. ) ;
#5648 = EDGE_CURVE ( 'NONE', #5726, #11314, #25435, .T. ) ;
#5649 = ORIENTED_EDGE ( 'NONE', *, *, #22948, .T. ) ;
#5650 = CARTESIAN_POINT ( 'NONE',  ( 30.81606138205700418, -39.60718113818700203, 83.30501292737011454 ) ) ;
#5651 = CARTESIAN_POINT ( 'NONE',  ( 33.56606138205700773, 41.44123852234599781, 75.30501292736988717 ) ) ;
#5652 = CARTESIAN_POINT ( 'NONE',  ( 40.52078840805428683, -18.61368208888610098, 70.60699637195608602 ) ) ;
#5653 = VECTOR ( 'NONE', #21399, 1000.000000000000000 ) ;
#5654 = EDGE_LOOP ( 'NONE', ( #19066, #1346, #20050, #20405 ) ) ;
#5655 = AXIS2_PLACEMENT_3D ( 'NONE', #21412, #11634, #14197 ) ;
#5656 = AXIS2_PLACEMENT_3D ( 'NONE', #207, #6277, #3957 ) ;
#5657 = DIRECTION ( 'NONE',  ( -1.000000000000000000, -2.751104698760144965E-15, 1.228345504986737969E-16 ) ) ;
#5658 = FACE_OUTER_BOUND ( 'NONE', #8760, .T. ) ;
#5659 = EDGE_CURVE ( 'NONE', #9093, #13053, #25312, .T. ) ;
#5660 = SURFACE_STYLE_USAGE ( .BOTH. , #25348 ) ;
#5661 = CARTESIAN_POINT ( 'NONE',  ( 36.81606138205700063, 6.191238522346988127, 65.30501292736998664 ) ) ;
#5662 = CARTESIAN_POINT ( 'NONE',  ( 37.31005363372398165, -5.470694883964326571, 83.30188305377672009 ) ) ;
#5663 = CARTESIAN_POINT ( 'NONE',  ( 37.25260217561390874, -10.00384086642191406, 70.97781676520604321 ) ) ;
#5664 = CARTESIAN_POINT ( 'NONE',  ( 39.51027997493896748, -28.51368208888610667, 71.32335560751960202 ) ) ;
#5665 = EDGE_LOOP ( 'NONE', ( #4858, #11044, #3195, #11714 ) ) ;
#5666 = CARTESIAN_POINT ( 'NONE',  ( 33.31606138205700773, 3.536347952325769040, 64.10938348997790115 ) ) ;
#5667 = EDGE_CURVE ( 'NONE', #4384, #18087, #11695, .T. ) ;
#5668 = DIRECTION ( 'NONE',  ( -1.000000000000000000, 0.000000000000000000, 0.000000000000000000 ) ) ;
#5669 = ORIENTED_EDGE ( 'NONE', *, *, #24235, .T. ) ;
#5670 = VECTOR ( 'NONE', #12137, 1000.000000000000000 ) ;
#5671 = VERTEX_POINT ( 'NONE', #19657 ) ;
#5672 = CARTESIAN_POINT ( 'NONE',  ( 40.77203464402485622, -27.10384086642191903, 71.43714994484031422 ) ) ;
#5673 = AXIS2_PLACEMENT_3D ( 'NONE', #24775, #15006, #16810 ) ;
#5674 = VECTOR ( 'NONE', #2647, 1000.000000000000000 ) ;
#5675 = CARTESIAN_POINT ( 'NONE',  ( 37.31647492878122563, -27.31368208888610027, 70.72433947564853440 ) ) ;
#5676 = CARTESIAN_POINT ( 'NONE',  ( 36.89935272106204422, -3.213682088886101962, 69.52238214136768590 ) ) ;
#5677 = ORIENTED_EDGE ( 'NONE', *, *, #20745, .T. ) ;
#5678 = DIRECTION ( 'NONE',  ( 0.000000000000000000, 0.3299742535180974490, -0.9439899321577398528 ) ) ;
#5679 = CARTESIAN_POINT ( 'NONE',  ( 38.73920764526923932, -7.503840866421911393, 70.26206559358664094 ) ) ;
#5680 = APPLICATION_CONTEXT ( 'automotive_design' ) ;
#5681 = DIRECTION ( 'NONE',  ( -1.000000000000000000, 5.204170427930413997E-31, 1.734723475976804876E-16 ) ) ;
#5682 = VERTEX_POINT ( 'NONE', #11946 ) ;
#5683 = DIRECTION ( 'NONE',  ( -2.478176394252580155E-16, 0.000000000000000000, -1.000000000000000000 ) ) ;
#5684 = DIRECTION ( 'NONE',  ( 1.836970198721029688E-16, 2.999999999999999839E-15, 1.000000000000000000 ) ) ;
#5685 = CARTESIAN_POINT ( 'NONE',  ( 36.98690846071097127, -9.803840866421911215, 69.45876917294177133 ) ) ;
#5686 = DIRECTION ( 'NONE',  ( -1.000000000000000000, 6.018531076210110289E-31, 1.734723475976804876E-16 ) ) ;
#5687 =( NAMED_UNIT ( * ) PLANE_ANGLE_UNIT ( ) SI_UNIT ( $, .RADIAN. ) );
#5688 = CARTESIAN_POINT ( 'NONE',  ( 39.98359781491296161, -16.41368208888610525, 71.86517103874047052 ) ) ;
#5689 = CARTESIAN_POINT ( 'NONE',  ( 31.81606138205700418, 38.19123852234599070, 72.05501292736988717 ) ) ;
#5690 = DIRECTION ( 'NONE',  ( 1.000000000000000000, 3.388898908187273079E-15, 1.919289851541777660E-16 ) ) ;
#5691 = ORIENTED_EDGE ( 'NONE', *, *, #5240, .T. ) ;
#5692 = VECTOR ( 'NONE', #332, 1000.000000000000000 ) ;
#5693 = DIRECTION ( 'NONE',  ( 2.011972697750612571E-15, -0.6595716529892353686, 0.7516416929448815898 ) ) ;
#5694 = CARTESIAN_POINT ( 'NONE',  ( 39.29254315202757653, -0.8038408664219134359, 72.81632618279323310 ) ) ;
#5695 = PRODUCT_CONTEXT ( 'NONE', #10953, 'mechanical' ) ;
#5696 = ADVANCED_FACE ( 'NONE', ( #3945 ), #1995, .T. ) ;
#5697 = CARTESIAN_POINT ( 'NONE',  ( 33.48677699869404023, 3.517612739349352591, 6.329933951274631099 ) ) ;
#5698 =( GEOMETRIC_REPRESENTATION_CONTEXT ( 3 ) GLOBAL_UNCERTAINTY_ASSIGNED_CONTEXT ( ( #685 ) ) GLOBAL_UNIT_ASSIGNED_CONTEXT ( ( #25478, #17647, #13522 ) ) REPRESENTATION_CONTEXT ( 'NONE', 'WORKASPACE' ) );
#5699 = CARTESIAN_POINT ( 'NONE',  ( 39.82603832034400426, -18.31368208888610738, 72.40698646996133903 ) ) ;
#5700 = EDGE_CURVE ( 'NONE', #24520, #19911, #11251, .T. ) ;
#5701 = LINE ( 'NONE', #11516, #12718 ) ;
#5702 = EDGE_CURVE ( 'NONE', #6796, #14420, #8073, .T. ) ;
#5703 = CIRCLE ( 'NONE', #20105, 1.249999999999996891 ) ;
#5704 = CARTESIAN_POINT ( 'NONE',  ( 37.33957961208645315, -17.80384086642190766, 69.94417936956672577 ) ) ;
#5705 = CARTESIAN_POINT ( 'NONE',  ( 36.72255525790973252, -5.951216915653229300, 82.77761203469431450 ) ) ;
#5706 = CARTESIAN_POINT ( 'NONE',  ( 37.33957961208646736, -19.81368208888611093, 72.81632618279321889 ) ) ;
#5707 = VERTEX_POINT ( 'NONE', #19918 ) ;
#5708 = CARTESIAN_POINT ( 'NONE',  ( 39.64521430340304420, -22.81368208888610383, 69.45876917294175712 ) ) ;
#5709 = VERTEX_POINT ( 'NONE', #10130 ) ;
#5710 = DIRECTION ( 'NONE',  ( 1.327674326049719602E-15, -0.4425581086832399147, 0.8967398287344627850 ) ) ;
#5711 = CARTESIAN_POINT ( 'NONE',  ( 44.81606138205700063, 35.44123852234597649, 68.80501292736990138 ) ) ;
#5712 = CARTESIAN_POINT ( 'NONE',  ( 39.41296390513587511, -27.20384086642191690, 71.08074471024438878 ) ) ;
#5713 = AXIS2_PLACEMENT_3D ( 'NONE', #12688, #806, #4691 ) ;
#5714 = ORIENTED_EDGE ( 'NONE', *, *, #10317, .F. ) ;
#5715 = ORIENTED_EDGE ( 'NONE', *, *, #348, .T. ) ;
#5716 = CARTESIAN_POINT ( 'NONE',  ( 39.59505955540748801, -28.75102279782487358, 70.48438567037749181 ) ) ;
#5717 = ADVANCED_FACE ( 'NONE', ( #17734 ), #8195, .T. ) ;
#5718 = LINE ( 'NONE', #19500, #13714 ) ;
#5719 = CARTESIAN_POINT ( 'NONE',  ( 38.37017380507018771, 0.3961591335780931256, 69.64448340153880679 ) ) ;
#5720 = CIRCLE ( 'NONE', #6949, 1.250000000000000888 ) ;
#5721 = LINE ( 'NONE', #13584, #23202 ) ;
#5722 = CARTESIAN_POINT ( 'NONE',  ( 39.73277004305198545, -4.213682088886105959, 73.23812341099225875 ) ) ;
#5723 = DIRECTION ( 'NONE',  ( 1.000000000000000000, 0.000000000000000000, 0.000000000000000000 ) ) ;
#5724 = ORIENTED_EDGE ( 'NONE', *, *, #3652, .F. ) ;
#5725 = VECTOR ( 'NONE', #19964, 1000.000000000000000 ) ;
#5726 = VERTEX_POINT ( 'NONE', #18245 ) ;
#5727 = CARTESIAN_POINT ( 'NONE',  ( 39.31606138205697931, -10.61256217995208040, 37.48782943861662886 ) ) ;
#5728 = CARTESIAN_POINT ( 'NONE',  ( 40.31606138205700773, -22.22127907754180853, 85.30501292736998664 ) ) ;
#5729 = CARTESIAN_POINT ( 'NONE',  ( 39.82603832034401137, -27.30384086642190766, 70.35351908239857721 ) ) ;
#5730 = SHAPE_REPRESENTATION_RELATIONSHIP ( 'NONE' , 'NONE' ,  #10983, #9253 ) ;
#5731 = CARTESIAN_POINT ( 'NONE',  ( 36.31606138205700063, -16.48551471403133206, 77.11349248448009064 ) ) ;
#5732 = VECTOR ( 'NONE', #11228, 1000.000000000000000 ) ;
#5733 = EDGE_LOOP ( 'NONE', ( #8462, #4043, #17220, #25215 ) ) ;
#5734 = DIRECTION ( 'NONE',  ( 0.000000000000000000, 0.4425581086832399702, -0.8967398287344626739 ) ) ;
#5735 = CARTESIAN_POINT ( 'NONE',  ( 33.31606138205700773, -5.204193249396356968, 72.80501292736992980 ) ) ;
#5736 = DIRECTION ( 'NONE',  ( -2.120312145707929538E-16, 0.8213699656732942334, -0.5703958094953462954 ) ) ;
#5737 = CARTESIAN_POINT ( 'NONE',  ( 37.25260217561390874, -4.003840866421911393, 70.97781676520604321 ) ) ;
#5738 = AXIS2_PLACEMENT_3D ( 'NONE', #19549, #10023, #18008 ) ;
#5739 = EDGE_LOOP ( 'NONE', ( #14750, #6008, #17895, #11523 ) ) ;
#5740 = DIRECTION ( 'NONE',  ( 1.000000000000000000, 0.000000000000000000, 0.000000000000000000 ) ) ;
#5741 = ORIENTED_EDGE ( 'NONE', *, *, #12746, .T. ) ;
#5742 = ORIENTED_EDGE ( 'NONE', *, *, #6302, .F. ) ;
#5743 = PLANE ( 'NONE',  #9374 ) ;
#5744 = VECTOR ( 'NONE', #24529, 1000.000000000000000 ) ;
#5745 = CARTESIAN_POINT ( 'NONE',  ( 38.93987200065208754, -12.81368208888610383, 70.42958956619168021 ) ) ;
#5746 = CARTESIAN_POINT ( 'NONE',  ( 38.73920764526925353, -12.11368208888610098, 72.49843995877330372 ) ) ;
#5747 = ORIENTED_EDGE ( 'NONE', *, *, #22486, .T. ) ;
#5748 = EDGE_LOOP ( 'NONE', ( #7015, #15333, #13534, #9275 ) ) ;
#5749 = CARTESIAN_POINT ( 'NONE',  ( 33.31606138205700773, -5.204193249396356968, 72.80501292736992980 ) ) ;
#5750 = EDGE_CURVE ( 'NONE', #16702, #5882, #443, .T. ) ;
#5751 = DIRECTION ( 'NONE',  ( 1.000000000000000000, 0.000000000000000000, 0.000000000000000000 ) ) ;
#5752 = ORIENTED_EDGE ( 'NONE', *, *, #3255, .F. ) ;
#5753 = CARTESIAN_POINT ( 'NONE',  ( 46.81606138205706458, -34.55876147768182705, 70.30501292735635843 ) ) ;
#5754 = CARTESIAN_POINT ( 'NONE',  ( 39.98359781491296161, -15.20384086642191157, 70.89533451361945993 ) ) ;
#5755 = VECTOR ( 'NONE', #21960, 1000.000000000000000 ) ;
#5756 = CARTESIAN_POINT ( 'NONE',  ( 42.71215467885433270, 2.748844572886082638, 6.091764642881028813 ) ) ;
#5757 = CARTESIAN_POINT ( 'NONE',  ( 37.38336156205274818, -21.71368208888610241, 72.12822762946750288 ) ) ;
#5758 = AXIS2_PLACEMENT_3D ( 'NONE', #2370, #12448, #18237 ) ;
#5759 = ORIENTED_EDGE ( 'NONE', *, *, #9428, .T. ) ;
#5760 = CARTESIAN_POINT ( 'NONE',  ( 31.81606138205700418, -38.55876147765410167, 70.30501292737011454 ) ) ;
#5761 = CIRCLE ( 'NONE', #13181, 2.000000000000001776 ) ;
#5762 = CARTESIAN_POINT ( 'NONE',  ( 39.98359781491296161, -12.41368208888610525, 71.86517103874047052 ) ) ;
#5763 = FACE_OUTER_BOUND ( 'NONE', #5064, .T. ) ;
#5764 = LINE ( 'NONE', #21346, #19430 ) ;
#5765 = VECTOR ( 'NONE', #9683, 1000.000000000000000 ) ;
#5766 = ADVANCED_FACE ( 'NONE', ( #8840 ), #4710, .F. ) ;
#5767 = EDGE_CURVE ( 'NONE', #18636, #23179, #2504, .T. ) ;
#5768 = CARTESIAN_POINT ( 'NONE',  ( 40.05520938202761982, -6.208431968299676917, 83.26252610654707098 ) ) ;
#5769 = CARTESIAN_POINT ( 'NONE',  ( 32.81606138205700773, -26.01295748837380373, 65.89261741282676610 ) ) ;
#5770 = CARTESIAN_POINT ( 'NONE',  ( 40.31606138205700773, -11.18542543036241987, 17.47151328161626793 ) ) ;
#5771 = EDGE_CURVE ( 'NONE', #19498, #5247, #20197, .T. ) ;
#5772 = ORIENTED_EDGE ( 'NONE', *, *, #2921, .F. ) ;
#5773 = DIRECTION ( 'NONE',  ( 0.000000000000000000, -0.6568589528324746407, 0.7540134720837717852 ) ) ;
#5774 = EDGE_LOOP ( 'NONE', ( #10503, #3832, #119, #5772 ) ) ;
#5775 = ORIENTED_EDGE ( 'NONE', *, *, #13038, .F. ) ;
#5776 = CARTESIAN_POINT ( 'NONE',  ( 37.61123632939164452, -7.703840866421914235, 69.02690120949094421 ) ) ;
#5777 = AXIS2_PLACEMENT_3D ( 'NONE', #6323, #16227, #17925 ) ;
#5778 = ORIENTED_EDGE ( 'NONE', *, *, #5032, .F. ) ;
#5779 = EDGE_CURVE ( 'NONE', #14211, #15541, #8580, .T. ) ;
#5780 = LINE ( 'NONE', #9780, #14072 ) ;
#5781 = CARTESIAN_POINT ( 'NONE',  ( 38.26194895904383486, -13.01368208888610134, 69.64448340153877837 ) ) ;
#5782 = VECTOR ( 'NONE', #23672, 1000.000000000000000 ) ;
#5783 = ORIENTED_EDGE ( 'NONE', *, *, #583, .F. ) ;
#5784 = LINE ( 'NONE', #19303, #5557 ) ;
#5785 = CARTESIAN_POINT ( 'NONE',  ( 38.41621794735363693, -38.10729675983899511, 84.30501292737011454 ) ) ;
#5786 = CARTESIAN_POINT ( 'NONE',  ( 36.89935272106204422, -19.21368208888609885, 69.52238214136768590 ) ) ;
#5787 = ORIENTED_EDGE ( 'NONE', *, *, #9395, .T. ) ;
#5788 = DIRECTION ( 'NONE',  ( 0.000000000000000000, -0.6568589528324746407, 0.7540134720837717852 ) ) ;
#5789 = CARTESIAN_POINT ( 'NONE',  ( 41.81606138205700063, -20.93319939328399926, 43.78741072286599945 ) ) ;
#5790 = CARTESIAN_POINT ( 'NONE',  ( 41.31606138205700063, 8.791238522312193382, 67.36094597237627113 ) ) ;
#5791 = PLANE ( 'NONE',  #19087 ) ;
#5792 = EDGE_CURVE ( 'NONE', #1915, #16335, #8452, .T. ) ;
#5793 = EDGE_CURVE ( 'NONE', #18040, #17256, #20008, .T. ) ;
#5794 = AXIS2_PLACEMENT_3D ( 'NONE', #23893, #6257, #24134 ) ;
#5795 = CARTESIAN_POINT ( 'NONE',  ( 43.81608638205700146, 0.9984178969752143251, 11.59873562314662010 ) ) ;
#5796 = EDGE_CURVE ( 'NONE', #2551, #22728, #23874, .T. ) ;
#5797 = CARTESIAN_POINT ( 'NONE',  ( 42.68042513965293949, 2.191238522347013440, 73.80501292737000085 ) ) ;
#5798 = AXIS2_PLACEMENT_3D ( 'NONE', #9249, #15022, #22878 ) ;
#5799 = EDGE_CURVE ( 'NONE', #9870, #24731, #12199, .T. ) ;
#5800 = CARTESIAN_POINT ( 'NONE',  ( 37.21915885897815457, -14.20384086642191335, 71.67976084211552745 ) ) ;
#5801 = CARTESIAN_POINT ( 'NONE',  ( 36.49096545463212493, 0.4863179111138959954, 71.43714994484035685 ) ) ;
#5802 = ADVANCED_FACE ( 'NONE', ( #8709 ), #6511, .T. ) ;
#5803 = VERTEX_POINT ( 'NONE', #4823 ) ;
#5804 = DIRECTION ( 'NONE',  ( -1.000000000000000000, 1.678764654171101651E-30, 5.595882180570339263E-16 ) ) ;
#5805 = CARTESIAN_POINT ( 'NONE',  ( 33.40064408022072939, 40.95934826813394380, 79.52109337493035923 ) ) ;
#5806 = VERTEX_POINT ( 'NONE', #22474 ) ;
#5807 = ORIENTED_EDGE ( 'NONE', *, *, #6965, .T. ) ;
#5808 = CARTESIAN_POINT ( 'NONE',  ( 38.26194895904384907, -0.6038408664219147015, 73.11602215082118050 ) ) ;
#5809 = EDGE_CURVE ( 'NONE', #14165, #19639, #14493, .T. ) ;
#5810 = CARTESIAN_POINT ( 'NONE',  ( 38.63098279924288647, -24.91368208888610170, 70.22690120949089021 ) ) ;
#5811 = CARTESIAN_POINT ( 'NONE',  ( 40.33642880535524000, -4.313682088886108268, 72.77780686321128201 ) ) ;
#5812 = ORIENTED_EDGE ( 'NONE', *, *, #20014, .T. ) ;
#5813 = LINE ( 'NONE', #17155, #8244 ) ;
#5814 = EDGE_CURVE ( 'NONE', #24859, #20881, #21850, .T. ) ;
#5815 = CARTESIAN_POINT ( 'NONE',  ( 39.31564783533279694, -3.303840866421912548, 70.72433947564853440 ) ) ;
#5816 = LINE ( 'NONE', #3741, #10181 ) ;
#5817 = ORIENTED_EDGE ( 'NONE', *, *, #23741, .F. ) ;
#5818 = DIRECTION ( 'NONE',  ( 1.000000000000000000, 0.000000000000000000, 0.000000000000000000 ) ) ;
#5819 = DIRECTION ( 'NONE',  ( 1.000000000000000000, 2.168404344971005170E-16, -1.734723475976814737E-16 ) ) ;
#5820 = CARTESIAN_POINT ( 'NONE',  ( 40.26954217208372455, -10.90384086642191974, 72.86986841596736042 ) ) ;
#5821 = DIRECTION ( 'NONE',  ( 0.000000000000000000, 1.000000000000000000, 0.000000000000000000 ) ) ;
#5822 = CARTESIAN_POINT ( 'NONE',  ( 39.38009889167650357, -14.21368208888610773, 72.75271321436731853 ) ) ;
#5823 = CARTESIAN_POINT ( 'NONE',  ( 34.06606138205700773, 3.151453266960317023, 6.397347472316774031 ) ) ;
#5824 = EDGE_CURVE ( 'NONE', #20600, #5217, #2905, .T. ) ;
#5825 = LINE ( 'NONE', #9325, #2732 ) ;
#5826 = CARTESIAN_POINT ( 'NONE',  ( 35.81606138205700063, 37.44123852234599781, 75.30501292736990138 ) ) ;
#5827 = CARTESIAN_POINT ( 'NONE',  ( 38.37017380507018771, -1.603840866421908595, 69.64448340153879258 ) ) ;
#5828 = CONTEXT_DEPENDENT_SHAPE_REPRESENTATION ( #3040, #12371 ) ;
#5829 = DIRECTION ( 'NONE',  ( 1.000000000000000000, 1.000000000000000078E-15, 0.000000000000000000 ) ) ;
#5830 = CARTESIAN_POINT ( 'NONE',  ( 37.69796330110504101, -19.11368208888610098, 69.66206559358661821 ) ) ;
#5831 = CARTESIAN_POINT ( 'NONE',  ( 36.06606138205695089, 2.967040633637572089, 4.322985289651505525 ) ) ;
#5832 = VECTOR ( 'NONE', #20451, 1000.000000000000000 ) ;
#5833 = CARTESIAN_POINT ( 'NONE',  ( 39.98359781491296161, -19.20384086642191335, 70.89533451361945993 ) ) ;
#5834 = FACE_OUTER_BOUND ( 'NONE', #13508, .T. ) ;
#5835 = CARTESIAN_POINT ( 'NONE',  ( 37.25202387243752611, -19.21368208888610241, 70.00779233799262613 ) ) ;
#5836 = ORIENTED_EDGE ( 'NONE', *, *, #24962, .T. ) ;
#5837 = CARTESIAN_POINT ( 'NONE',  ( 38.26194895904383486, -19.01368208888609956, 69.04448340153878405 ) ) ;
#5838 = ORIENTED_EDGE ( 'NONE', *, *, #7644, .F. ) ;
#5839 = PLANE ( 'NONE',  #4530 ) ;
#5840 = CARTESIAN_POINT ( 'NONE',  ( 36.31606138205702194, -20.48251210171517300, 31.50167136002490764 ) ) ;
#5841 = CARTESIAN_POINT ( 'NONE',  ( 38.63098279924290068, -22.70384086642191335, 72.53360434286904024 ) ) ;
#5842 = ORIENTED_EDGE ( 'NONE', *, *, #1081, .T. ) ;
#5843 = ORIENTED_EDGE ( 'NONE', *, *, #9409, .T. ) ;
#5844 = PLANE ( 'NONE',  #5130 ) ;
#5845 = PLANE ( 'NONE',  #14536 ) ;
#5846 = EDGE_LOOP ( 'NONE', ( #20851, #4576, #24705, #14519 ) ) ;
#5847 = CARTESIAN_POINT ( 'NONE',  ( 33.31606138205700773, 7.043113989679085307, 66.83274420321491505 ) ) ;
#5848 = CARTESIAN_POINT ( 'NONE',  ( 39.82603832034400426, -1.303840866421906997, 70.35351908239857721 ) ) ;
#5849 = EDGE_CURVE ( 'NONE', #17790, #13140, #14247, .T. ) ;
#5850 = ADVANCED_FACE ( 'NONE', ( #20415 ), #24392, .T. ) ;
#5851 = CARTESIAN_POINT ( 'NONE',  ( 31.81606138205700418, 34.87886987267149408, 80.75501292736984738 ) ) ;
#5852 = CARTESIAN_POINT ( 'NONE',  ( 36.36258059203031934, 0.2863179111138938193, 72.86986841596736042 ) ) ;
#5853 = PRODUCT_RELATED_PRODUCT_CATEGORY ( 'part', '', ( #17752 ) ) ;
#5854 = CIRCLE ( 'NONE', #7484, 1.000000000000000888 ) ;
#5855 = DIRECTION ( 'NONE',  ( -1.000000000000000000, 0.000000000000000000, 0.000000000000000000 ) ) ;
#5856 = AXIS2_PLACEMENT_3D ( 'NONE', #6674, #14166, #22014 ) ;
#5857 = VERTEX_POINT ( 'NONE', #690 ) ;
#5858 = ORIENTED_EDGE ( 'NONE', *, *, #8001, .F. ) ;
#5859 = CARTESIAN_POINT ( 'NONE',  ( 31.81606138205700418, -26.74044063519544778, 66.30501292737000085 ) ) ;
#5860 = FACE_OUTER_BOUND ( 'NONE', #191, .T. ) ;
#5861 = CIRCLE ( 'NONE', #16526, 0.5000000000000004441 ) ;
#5862 = CARTESIAN_POINT ( 'NONE',  ( 36.68196826583682935, -22.00384086642191406, 70.79240656858107172 ) ) ;
#5863 = CYLINDRICAL_SURFACE ( 'NONE', #8364, 4.000000000000003553 ) ;
#5864 = VERTEX_POINT ( 'NONE', #10639 ) ;
#5865 = LINE ( 'NONE', #20023, #9019 ) ;
#5866 = AXIS2_PLACEMENT_3D ( 'NONE', #4367, #2167, #4118 ) ;
#5867 = LINE ( 'NONE', #12185, #11122 ) ;
#5868 = LINE ( 'NONE', #3934, #5238 ) ;
#5869 = CARTESIAN_POINT ( 'NONE',  ( 37.12184278917507640, -4.103840866421911038, 71.32335560751961623 ) ) ;
#5870 = VERTEX_POINT ( 'NONE', #823 ) ;
#5871 = FACE_OUTER_BOUND ( 'NONE', #10353, .T. ) ;
#5872 = ORIENTED_EDGE ( 'NONE', *, *, #19057, .T. ) ;
#5873 = VERTEX_POINT ( 'NONE', #6766 ) ;
#5874 = CIRCLE ( 'NONE', #1320, 1.499999999999999778 ) ;
#5875 = CARTESIAN_POINT ( 'NONE',  ( 34.56606138205700773, 47.04446929126254417, 81.37823623207319201 ) ) ;
#5876 = CARTESIAN_POINT ( 'NONE',  ( 38.26194895904383486, -13.01368208888610312, 70.24448340153875847 ) ) ;
#5877 = CARTESIAN_POINT ( 'NONE',  ( 39.02742774030102879, -12.21368208888610063, 72.26730301774234988 ) ) ;
#5878 = EDGE_LOOP ( 'NONE', ( #11010, #19176, #7935, #24324 ) ) ;
#5879 = ORIENTED_EDGE ( 'NONE', *, *, #17907, .T. ) ;
#5880 = CARTESIAN_POINT ( 'NONE',  ( 36.31606138205700063, -16.77230293220685198, 77.52306850662458260 ) ) ;
#5881 = CARTESIAN_POINT ( 'NONE',  ( 32.81606138205700773, 35.44123852234597649, 68.80501292736990138 ) ) ;
#5882 = VERTEX_POINT ( 'NONE', #14618 ) ;
#5883 = CARTESIAN_POINT ( 'NONE',  ( 43.81606138205700063, 41.44123852234599070, 73.05501292736987295 ) ) ;
#5884 = CARTESIAN_POINT ( 'NONE',  ( 37.25202387243754032, -20.40384086642191619, 72.75271321436731853 ) ) ;
#5885 = ADVANCED_FACE ( 'NONE', ( #19239 ), #13768, .T. ) ;
#5886 = LINE ( 'NONE', #7693, #23529 ) ;
#5887 = CIRCLE ( 'NONE', #25198, 1.750000000000001776 ) ;
#5888 = CYLINDRICAL_SURFACE ( 'NONE', #12884, 0.7500000000000001110 ) ;
#5889 = CARTESIAN_POINT ( 'NONE',  ( 39.31564783533280405, -18.31368208888610027, 72.03616607671141026 ) ) ;
#5890 = ORIENTED_EDGE ( 'NONE', *, *, #5424, .T. ) ;
#5891 = ORIENTED_EDGE ( 'NONE', *, *, #22166, .F. ) ;
#5892 = DIRECTION ( 'NONE',  ( -1.000000000000000000, -2.999999999999999839E-15, 0.000000000000000000 ) ) ;
#5893 = CARTESIAN_POINT ( 'NONE',  ( 38.26194895904383486, -11.01368208888609956, 69.64448340153879258 ) ) ;
#5894 = VECTOR ( 'NONE', #3638, 1000.000000000000000 ) ;
#5895 = DIRECTION ( 'NONE',  ( 0.000000000000000000, 2.999999999999999839E-15, 1.000000000000000000 ) ) ;
#5896 = VECTOR ( 'NONE', #19766, 1000.000000000000000 ) ;
#5897 = DIRECTION ( 'NONE',  ( 1.000000000000000000, -0.000000000000000000, 0.000000000000000000 ) ) ;
#5898 = PLANE ( 'NONE',  #6546 ) ;
#5899 = DIRECTION ( 'NONE',  ( -1.734723475976814737E-16, 1.000000000000000000, -3.491481338843135327E-15 ) ) ;
#5900 = EDGE_CURVE ( 'NONE', #11164, #24520, #21058, .T. ) ;
#5901 = AXIS2_PLACEMENT_3D ( 'NONE', #15760, #23350, #23619 ) ;
#5902 = CARTESIAN_POINT ( 'NONE',  ( 43.69896204258590444, 3.548173818309678484, 6.215045287937394747 ) ) ;
#5903 = TOROIDAL_SURFACE ( 'NONE', #17027, 0.9023161253044896801, 0.2000000000000000111 ) ;
#5904 = DIRECTION ( 'NONE',  ( -1.000000000000000000, 0.000000000000000000, 0.000000000000000000 ) ) ;
#5905 = ORIENTED_EDGE ( 'NONE', *, *, #12960, .T. ) ;
#5906 = ORIENTED_EDGE ( 'NONE', *, *, #2081, .T. ) ;
#5907 = PRODUCT_DEFINITION_CONTEXT ( 'detailed design', #739, 'design' ) ;
#5908 = CARTESIAN_POINT ( 'NONE',  ( 36.89935272106205133, -6.403840866421917077, 73.23812341099225875 ) ) ;
#5909 = VERTEX_POINT ( 'NONE', #13208 ) ;
#5910 = DIRECTION ( 'NONE',  ( -1.000000000000000000, 1.040834085586084551E-30, 3.469446951953615175E-16 ) ) ;
#5911 = CARTESIAN_POINT ( 'NONE',  ( 36.80608444377001121, -15.31368208888610383, 70.35351908239857721 ) ) ;
#5912 = AXIS2_PLACEMENT_3D ( 'NONE', #9580, #1687, #9454 ) ;
#5913 = ORIENTED_EDGE ( 'NONE', *, *, #21686, .T. ) ;
#5914 = DIRECTION ( 'NONE',  ( 1.000000000000000000, 0.000000000000000000, 0.000000000000000000 ) ) ;
#5915 = DIRECTION ( 'NONE',  ( 1.000000000000000000, 2.999999999999999839E-15, 0.000000000000000000 ) ) ;
#5916 = VECTOR ( 'NONE', #13547, 1000.000000000000000 ) ;
#5917 = CARTESIAN_POINT ( 'NONE',  ( 39.12911128074873801, -12.11368208888610987, 73.69843995877327814 ) ) ;
#5918 = ORIENTED_EDGE ( 'NONE', *, *, #19977, .F. ) ;
#5919 = PLANE ( 'NONE',  #20095 ) ;
#5920 = LINE ( 'NONE', #3593, #914 ) ;
#5921 = VECTOR ( 'NONE', #4800, 1000.000000000000000 ) ;
#5922 = FACE_OUTER_BOUND ( 'NONE', #9575, .T. ) ;
#5923 = CARTESIAN_POINT ( 'NONE',  ( 43.23147868389327897, 42.57231754924293909, 79.37823623207320622 ) ) ;
#5924 = EDGE_CURVE ( 'NONE', #20215, #13311, #3048, .T. ) ;
#5925 = AXIS2_PLACEMENT_3D ( 'NONE', #7171, #13095, #20823 ) ;
#5926 = CARTESIAN_POINT ( 'NONE',  ( 32.81606138205700773, 2.740850673309605412, 6.112030963703427133 ) ) ;
#5927 = CARTESIAN_POINT ( 'NONE',  ( 39.37952058850012804, -11.00384086642191050, 71.78268878715392987 ) ) ;
#5928 = CARTESIAN_POINT ( 'NONE',  ( 37.69796330110504101, -1.113682088886101207, 69.66206559358663242 ) ) ;
#5929 = VERTEX_POINT ( 'NONE', #18742 ) ;
#5930 = DIRECTION ( 'NONE',  ( -1.000000000000000000, 0.000000000000000000, 0.000000000000000000 ) ) ;
#5931 = AXIS2_PLACEMENT_3D ( 'NONE', #23290, #21123, #3468 ) ;
#5932 = CARTESIAN_POINT ( 'NONE',  ( 38.31606138205696510, -3.195232061939692336, -6.457771442202879797 ) ) ;
#5933 = ORIENTED_EDGE ( 'NONE', *, *, #14978, .F. ) ;
#5934 = VERTEX_POINT ( 'NONE', #12954 ) ;
#5935 = CARTESIAN_POINT ( 'NONE',  ( 38.82593461698265003, 1.296159133578084210, 73.13360434286906298 ) ) ;
#5936 = CARTESIAN_POINT ( 'NONE',  ( 37.25260217561390874, -25.61368208888610098, 71.78268878715390144 ) ) ;
#5937 = CARTESIAN_POINT ( 'NONE',  ( 40.55423172469004811, -2.413682088886103472, 72.05058123536544201 ) ) ;
#5938 = VERTEX_POINT ( 'NONE', #17191 ) ;
#5939 = LINE ( 'NONE', #9811, #811 ) ;
#5940 = CARTESIAN_POINT ( 'NONE',  ( 39.82603832034400426, -29.30384086642190766, 70.35351908239857721 ) ) ;
#5941 = EDGE_CURVE ( 'NONE', #22555, #9175, #22468, .T. ) ;
#5942 = CYLINDRICAL_SURFACE ( 'NONE', #11871, 1.000000000000000888 ) ;
#5943 = ADVANCED_FACE ( 'NONE', ( #11398 ), #25017, .T. ) ;
#5944 = ORIENTED_EDGE ( 'NONE', *, *, #16642, .T. ) ;
#5945 = DIRECTION ( 'NONE',  ( -7.292888252353849301E-16, 0.000000000000000000, 1.000000000000000000 ) ) ;
#5946 = PLANE ( 'NONE',  #14547 ) ;
#5947 = CARTESIAN_POINT ( 'NONE',  ( 40.77203464402485622, -9.103840866421915479, 71.43714994484034264 ) ) ;
#5948 = EDGE_CURVE ( 'NONE', #11106, #12188, #19927, .T. ) ;
#5949 = CIRCLE ( 'NONE', #10050, 0.7500000000000006661 ) ;
#5950 = EDGE_CURVE ( 'NONE', #20277, #20897, #15252, .T. ) ;
#5951 = EDGE_CURVE ( 'NONE', #20177, #17565, #11012, .T. ) ;
#5952 = LINE ( 'NONE', #23454, #18509 ) ;
#5953 = CARTESIAN_POINT ( 'NONE',  ( 38.93415946300897446, -12.11368208888610276, 73.09843995877329803 ) ) ;
#5954 = CARTESIAN_POINT ( 'NONE',  ( 37.31606138205702194, -20.48251210171516590, 31.50167136002490764 ) ) ;
#5955 = CIRCLE ( 'NONE', #24033, 3.000000000000002220 ) ;
#5956 = CARTESIAN_POINT ( 'NONE',  ( 39.38009889167650357, -26.21368208888610951, 72.75271321436730432 ) ) ;
#5957 = CARTESIAN_POINT ( 'NONE',  ( 30.81606138205697576, -4.349482454670884124, -5.142398479549302515 ) ) ;
#5958 = ADVANCED_FACE ( 'NONE', ( #20931 ), #4958, .F. ) ;
#5959 = CARTESIAN_POINT ( 'NONE',  ( 39.95015449827720744, 0.9961591335780894951, 71.96809898377890136 ) ) ;
#5960 = ADVANCED_FACE ( 'NONE', ( #1206 ), #23102, .F. ) ;
#5961 = DIRECTION ( 'NONE',  ( 0.000000000000000000, -0.3299742535180974490, 0.9439899321577398528 ) ) ;
#5962 = CARTESIAN_POINT ( 'NONE',  ( 39.75915168707250302, -18.71368208888610241, 70.26145752964251301 ) ) ;
#5963 = FACE_OUTER_BOUND ( 'NONE', #23640, .T. ) ;
#5964 = CARTESIAN_POINT ( 'NONE',  ( 37.25202387243754032, -16.40384086642191619, 72.75271321436731853 ) ) ;
#5965 = CARTESIAN_POINT ( 'NONE',  ( 44.81606138205700063, 36.92314894770293421, 79.37823623207323465 ) ) ;
#5966 = ADVANCED_FACE ( 'NONE', ( #15122 ), #12826, .T. ) ;
#5967 = CARTESIAN_POINT ( 'NONE',  ( 38.93415946300897446, -10.11368208888610987, 73.09843995877331224 ) ) ;
#5968 = EDGE_LOOP ( 'NONE', ( #20132, #9383, #11486, #17134 ) ) ;
#5969 = CARTESIAN_POINT ( 'NONE',  ( 36.29569395875879678, -23.31368208888610383, 69.98269868914866265 ) ) ;
#5970 = ORIENTED_EDGE ( 'NONE', *, *, #6000, .T. ) ;
#5971 = CARTESIAN_POINT ( 'NONE',  ( 44.81606138205700063, -31.45856502260510013, 77.07494475056050476 ) ) ;
#5972 = LINE ( 'NONE', #21297, #24381 ) ;
#5973 = CARTESIAN_POINT ( 'NONE',  ( 39.51027997493896748, -17.10384086642191193, 71.43714994484032843 ) ) ;
#5974 = ORIENTED_EDGE ( 'NONE', *, *, #22310, .F. ) ;
#5975 = ORIENTED_EDGE ( 'NONE', *, *, #12960, .F. ) ;
#5976 = LINE ( 'NONE', #13956, #16211 ) ;
#5977 = CARTESIAN_POINT ( 'NONE',  ( 38.31606138205696510, -1.965028424401967344, 1.888915691893686244 ) ) ;
#5978 = ORIENTED_EDGE ( 'NONE', *, *, #13903, .F. ) ;
#5979 = DIRECTION ( 'NONE',  ( -1.849283715844614702E-16, 0.8212051873014210024, 0.5706330172266920187 ) ) ;
#5980 = CARTESIAN_POINT ( 'NONE',  ( 38.26194895904384907, 1.396159133578083633, 73.11602215082119471 ) ) ;
#5981 = CARTESIAN_POINT ( 'NONE',  ( 59.50607210797845426, 32.97469880962110267, 84.30501292736985874 ) ) ;
#5982 = CARTESIAN_POINT ( 'NONE',  ( 36.89935272106204422, -3.213682088886101962, 69.52238214136768590 ) ) ;
#5983 = DIRECTION ( 'NONE',  ( 0.000000000000000000, -0.8212051873014208914, -0.5706330172266919076 ) ) ;
#5984 = VECTOR ( 'NONE', #6568, 1000.000000000000000 ) ;
#5985 = ORIENTED_EDGE ( 'NONE', *, *, #3106, .F. ) ;
#5986 = ORIENTED_EDGE ( 'NONE', *, *, #2797, .F. ) ;
#5987 = DIRECTION ( 'NONE',  ( 0.000000000000000000, -0.7540134720837697868, -0.6568589528324768612 ) ) ;
#5988 = CARTESIAN_POINT ( 'NONE',  ( 46.81606138205697221, -4.349482454670835274, -5.142398479549302515 ) ) ;
#5989 = EDGE_CURVE ( 'NONE', #23131, #10242, #24767, .T. ) ;
#5990 = CARTESIAN_POINT ( 'NONE',  ( 39.82603832034401137, -23.30384086642190766, 70.35351908239857721 ) ) ;
#5991 = SURFACE_STYLE_FILL_AREA ( #175 ) ;
#5992 = CARTESIAN_POINT ( 'NONE',  ( 30.81606138205697931, -3.863943790789087895, -7.177613496534175574 ) ) ;
#5993 = ORIENTED_EDGE ( 'NONE', *, *, #20604, .F. ) ;
#5994 = DIRECTION ( 'NONE',  ( 1.000000000000000000, -1.115179377413661005E-30, -3.717264591378870232E-16 ) ) ;
#5995 = DIRECTION ( 'NONE',  ( 8.758115402030106693E-47, -1.000000000000000000, 3.469446951953613400E-15 ) ) ;
#5996 = ORIENTED_EDGE ( 'NONE', *, *, #24590, .T. ) ;
#5997 = CARTESIAN_POINT ( 'NONE',  ( 39.24876120206129571, -4.903840866421912636, 72.12822762946750288 ) ) ;
#5998 = DIRECTION ( 'NONE',  ( -1.734723475976804876E-16, -3.491481338843135327E-15, -1.000000000000000000 ) ) ;
#5999 = ORIENTED_EDGE ( 'NONE', *, *, #21334, .F. ) ;
#6000 = EDGE_CURVE ( 'NONE', #10377, #3314, #16803, .T. ) ;
#6001 = CARTESIAN_POINT ( 'NONE',  ( 36.31606138205700773, -18.80550481115971451, 25.27912300651437150 ) ) ;
#6002 = ORIENTED_EDGE ( 'NONE', *, *, #9428, .F. ) ;
#6003 = ORIENTED_EDGE ( 'NONE', *, *, #24575, .F. ) ;
#6004 = CARTESIAN_POINT ( 'NONE',  ( 43.31606138205700063, -22.22127907754187959, 75.30501292736998664 ) ) ;
#6005 = CARTESIAN_POINT ( 'NONE',  ( 39.51027997493896748, -10.51368208888610134, 71.32335560751961623 ) ) ;
#6006 = CARTESIAN_POINT ( 'NONE',  ( 39.02742774030102879, -10.21368208888610241, 72.26730301774236409 ) ) ;
#6007 = ORIENTED_EDGE ( 'NONE', *, *, #12104, .T. ) ;
#6008 = ORIENTED_EDGE ( 'NONE', *, *, #18535, .F. ) ;
#6009 = CARTESIAN_POINT ( 'NONE',  ( 43.31606138205700063, -10.93995761290683255, 80.99653337025984001 ) ) ;
#6010 = CARTESIAN_POINT ( 'NONE',  ( 32.82453666081570276, -33.17626767724735259, 59.69730752409159180 ) ) ;
#6011 = ORIENTED_EDGE ( 'NONE', *, *, #7366, .T. ) ;
#6012 = DIRECTION ( 'NONE',  ( 0.000000000000000000, 0.8967398287344626739, 0.4425581086832399147 ) ) ;
#6013 = CARTESIAN_POINT ( 'NONE',  ( 36.64852494920107517, -16.20384086642190979, 71.86517103874048473 ) ) ;
#6014 = DIRECTION ( 'NONE',  ( 1.000000000000000000, 2.490066548941357028E-15, 1.228895056384528999E-15 ) ) ;
#6015 = CARTESIAN_POINT ( 'NONE',  ( 46.81606138205705747, -32.32696853385078128, 75.83798663122490780 ) ) ;
#6016 = CARTESIAN_POINT ( 'NONE',  ( 38.00113996487114321, -15.91368208888609992, 72.53360434286904024 ) ) ;
#6017 = ORIENTED_EDGE ( 'NONE', *, *, #17300, .T. ) ;
#6018 = ORIENTED_EDGE ( 'NONE', *, *, #3254, .T. ) ;
#6019 = LINE ( 'NONE', #6521, #18250 ) ;
#6020 = CARTESIAN_POINT ( 'NONE',  ( 39.82603832034401847, -14.31368208888610738, 72.40698646996131060 ) ) ;
#6021 = CYLINDRICAL_SURFACE ( 'NONE', #19673, 4.000000000000000000 ) ;
#6022 = FACE_OUTER_BOUND ( 'NONE', #4459, .T. ) ;
#6023 = VECTOR ( 'NONE', #14060, 1000.000000000000000 ) ;
#6024 = CARTESIAN_POINT ( 'NONE',  ( 43.31606138205700063, -35.82531359714782582, 71.25150419970752580 ) ) ;
#6025 = CARTESIAN_POINT ( 'NONE',  ( 40.07112981125872864, -29.10876147765398869, 71.40768163349989095 ) ) ;
#6026 = EDGE_CURVE ( 'NONE', #5120, #25303, #14864, .T. ) ;
#6027 = DIRECTION ( 'NONE',  ( 0.000000000000000000, 1.000000000000000000, -2.999999999999999839E-15 ) ) ;
#6028 = CARTESIAN_POINT ( 'NONE',  ( 31.81606138205700418, 39.39281886181299797, 81.75501292736984738 ) ) ;
#6029 = APPLICATION_CONTEXT ( 'automotive_design' ) ;
#6030 = EDGE_CURVE ( 'NONE', #16125, #20225, #5215, .T. ) ;
#6031 = ORIENTED_EDGE ( 'NONE', *, *, #20435, .T. ) ;
#6032 = EDGE_CURVE ( 'NONE', #13165, #14570, #13077, .T. ) ;
#6033 = CARTESIAN_POINT ( 'NONE',  ( 45.81606138205697931, -6.548589660139387369, -8.069948661059591188 ) ) ;
#6034 = VERTEX_POINT ( 'NONE', #1337 ) ;
#6035 = ORIENTED_EDGE ( 'NONE', *, *, #17103, .F. ) ;
#6036 = CARTESIAN_POINT ( 'NONE',  ( 38.37017380507018771, -3.603840866421911038, 69.04448340153881247 ) ) ;
#6037 = ORIENTED_EDGE ( 'NONE', *, *, #24840, .T. ) ;
#6038 = CARTESIAN_POINT ( 'NONE',  ( 31.81606138205700418, -34.55876147765401640, 70.30501292737011454 ) ) ;
#6039 = CARTESIAN_POINT ( 'NONE',  ( 38.82593461698262871, -6.913682088886100807, 69.62690120949091011 ) ) ;
#6040 = EDGE_LOOP ( 'NONE', ( #6384, #1871 ) ) ;
#6041 = FACE_OUTER_BOUND ( 'NONE', #21430, .T. ) ;
#6042 = EDGE_CURVE ( 'NONE', #18207, #14131, #11658, .T. ) ;
#6043 = CARTESIAN_POINT ( 'NONE',  ( 40.52078840805428683, -16.61368208888610454, 70.60699637195608602 ) ) ;
#6044 = CARTESIAN_POINT ( 'NONE',  ( 44.31606138205700063, 10.06218483883314718, 67.80501292737497465 ) ) ;
#6045 = DIRECTION ( 'NONE',  ( -1.000000000000000000, 0.000000000000000000, 0.000000000000000000 ) ) ;
#6046 = CIRCLE ( 'NONE', #20442, 2.500000000000002220 ) ;
#6047 = FACE_OUTER_BOUND ( 'NONE', #5504, .T. ) ;
#6048 =( LENGTH_UNIT ( ) NAMED_UNIT ( * ) SI_UNIT ( .MILLI., .METRE. ) );
#6049 = AXIS2_PLACEMENT_3D ( 'NONE', #21576, #3657, #21196 ) ;
#6050 = AXIS2_PLACEMENT_3D ( 'NONE', #8915, #22301, #12912 ) ;
#6051 = CARTESIAN_POINT ( 'NONE',  ( 43.81606138205700063, -24.55876147765400574, 72.80501292737008612 ) ) ;
#6052 = DIRECTION ( 'NONE',  ( 1.000000000000000000, -2.616121358439845201E-18, 3.764893311995947332E-18 ) ) ;
#6053 = DIRECTION ( 'NONE',  ( -9.027796614315171564E-31, -1.000000000000000000, -1.163336342344335610E-15 ) ) ;
#6054 = CARTESIAN_POINT ( 'NONE',  ( 38.00113996487114321, -25.91368208888609814, 72.53360434286901182 ) ) ;
#6055 = ORIENTED_EDGE ( 'NONE', *, *, #23872, .T. ) ;
#6056 = DIRECTION ( 'NONE',  ( 0.000000000000000000, -4.625929269271481378E-15, -1.000000000000000000 ) ) ;
#6057 = FACE_OUTER_BOUND ( 'NONE', #21026, .T. ) ;
#6058 = ORIENTED_EDGE ( 'NONE', *, *, #5659, .T. ) ;
#6059 = ORIENTED_EDGE ( 'NONE', *, *, #13143, .F. ) ;
#6060 = CARTESIAN_POINT ( 'NONE',  ( 36.98690846071097127, -21.80384086642191122, 69.45876917294175712 ) ) ;
#6061 = CARTESIAN_POINT ( 'NONE',  ( 39.37952058850012804, -24.61368208888610454, 70.97781676520600058 ) ) ;
#6062 = CARTESIAN_POINT ( 'NONE',  ( 40.14115730948191185, -24.51368208888609601, 71.32335560751958781 ) ) ;
#6063 = ORIENTED_EDGE ( 'NONE', *, *, #23181, .T. ) ;
#6064 = DIRECTION ( 'NONE',  ( 1.000000000000000000, 8.911169920151748851E-16, 3.114923731923493702E-16 ) ) ;
#6065 = CARTESIAN_POINT ( 'NONE',  ( 39.37952058850012804, 0.9961591335780894951, 71.78268878715394408 ) ) ;
#6066 = VECTOR ( 'NONE', #18845, 1000.000000000000000 ) ;
#6067 = CIRCLE ( 'NONE', #12660, 1.750000000000001554 ) ;
#6068 = CARTESIAN_POINT ( 'NONE',  ( -3.469446951953610245E-16, 45.92314894770294131, 80.37823623207322044 ) ) ;
#6069 = ORIENTED_EDGE ( 'NONE', *, *, #9737, .T. ) ;
#6070 = PLANE ( 'NONE',  #6396 ) ;
#6071 = CARTESIAN_POINT ( 'NONE',  ( 44.31606138205700063, 10.06218483883314718, 67.80501292737497465 ) ) ;
#6072 = EDGE_CURVE ( 'NONE', #12980, #5934, #23617, .T. ) ;
#6073 = CARTESIAN_POINT ( 'NONE',  ( 40.55423172469004101, -5.203840866421914235, 70.70992431699450265 ) ) ;
#6074 = CARTESIAN_POINT ( 'NONE',  ( 36.31606138205700063, -13.36080775159014244, 37.40752645450730540 ) ) ;
#6075 = DIRECTION ( 'NONE',  ( -1.000000000000000000, -2.999999999999999839E-15, 0.000000000000000000 ) ) ;
#6076 = CARTESIAN_POINT ( 'NONE',  ( 37.25202387243752611, -5.213682088886100630, 70.00779233799264034 ) ) ;
#6077 = LINE ( 'NONE', #3887, #22415 ) ;
#6078 = CARTESIAN_POINT ( 'NONE',  ( 37.80618814713140097, -27.91368208888610880, 73.13360434286902034 ) ) ;
#6079 = FACE_OUTER_BOUND ( 'NONE', #8197, .T. ) ;
#6080 = CARTESIAN_POINT ( 'NONE',  ( 38.37017380507018771, -3.603840866421907041, 69.64448340153879258 ) ) ;
#6081 = VECTOR ( 'NONE', #10403, 1000.000000000000000 ) ;
#6082 = DIRECTION ( 'NONE',  ( -1.000000000000000000, 0.000000000000000000, 0.000000000000000000 ) ) ;
#6083 = EDGE_CURVE ( 'NONE', #6422, #12591, #5976, .T. ) ;
#6084 = CARTESIAN_POINT ( 'NONE',  ( 39.38009889167650357, -10.21368208888610773, 72.75271321436733274 ) ) ;
#6085 = VECTOR ( 'NONE', #22776, 1000.000000000000000 ) ;
#6086 = EDGE_CURVE ( 'NONE', #22567, #10123, #22398, .T. ) ;
#6087 = CARTESIAN_POINT ( 'NONE',  ( 32.81606138205700773, -33.70281195181703993, 69.07320514641659770 ) ) ;
#6088 = CARTESIAN_POINT ( 'NONE',  ( 36.68196826583682935, -12.00384086642191228, 70.79240656858107172 ) ) ;
#6089 = ADVANCED_FACE ( 'NONE', ( #21684 ), #1960, .T. ) ;
#6090 = CARTESIAN_POINT ( 'NONE',  ( 46.81606138205701484, -19.40517585842700043, 23.66972737280834238 ) ) ;
#6091 = CARTESIAN_POINT ( 'NONE',  ( 38.26194895904383486, -11.01368208888609956, 69.64448340153879258 ) ) ;
#6092 = ORIENTED_EDGE ( 'NONE', *, *, #15709, .F. ) ;
#6093 = CARTESIAN_POINT ( 'NONE',  ( 36.89935272106204422, -19.21368208888609885, 69.52238214136768590 ) ) ;
#6094 = ORIENTED_EDGE ( 'NONE', *, *, #9587, .T. ) ;
#6095 = DIRECTION ( 'NONE',  ( 0.000000000000000000, 0.7540134720837716742, 0.6568589528324746407 ) ) ;
#6096 = CARTESIAN_POINT ( 'NONE',  ( 39.24876120206129571, -20.90384086642191264, 72.12822762946747446 ) ) ;
#6097 = ORIENTED_EDGE ( 'NONE', *, *, #583, .T. ) ;
#6098 = ORIENTED_EDGE ( 'NONE', *, *, #4521, .F. ) ;
#6099 = DIRECTION ( 'NONE',  ( -1.000000000000000000, -3.469446951953611033E-15, 0.000000000000000000 ) ) ;
#6100 = DIRECTION ( 'NONE',  ( 0.000000000000000000, -2.999999999999999839E-15, -1.000000000000000000 ) ) ;
#6101 = ADVANCED_FACE ( 'NONE', ( #15759 ), #4172, .T. ) ;
#6102 = CARTESIAN_POINT ( 'NONE',  ( 40.33642880535521869, -21.30384086642190766, 69.98269868914866265 ) ) ;
#6103 = CIRCLE ( 'NONE', #15961, 1.500000000000001332 ) ;
#6104 = DIRECTION ( 'NONE',  ( 2.312964634635740294E-15, 2.999999999999999839E-15, 1.000000000000000000 ) ) ;
#6105 = CARTESIAN_POINT ( 'NONE',  ( 36.89935272106204422, 0.7863179111138978161, 69.52238214136768590 ) ) ;
#6106 = DIRECTION ( 'NONE',  ( 1.000000000000000000, 1.734723475976804876E-16, -1.734723475976814737E-16 ) ) ;
#6107 = ORIENTED_EDGE ( 'NONE', *, *, #23872, .F. ) ;
#6108 = ORIENTED_EDGE ( 'NONE', *, *, #24822, .T. ) ;
#6109 = CARTESIAN_POINT ( 'NONE',  ( 33.48762233684214351, 2.904852044443344106, 6.096108814113431862 ) ) ;
#6110 = DIRECTION ( 'NONE',  ( -1.000000000000000000, 1.040834085586084551E-30, 3.469446951953615175E-16 ) ) ;
#6111 = CARTESIAN_POINT ( 'NONE',  ( 39.82603832034401137, -19.30384086642190411, 70.35351908239857721 ) ) ;
#6112 = PRESENTATION_STYLE_ASSIGNMENT (( #14098 ) ) ;
#6113 = LINE ( 'NONE', #19900, #18630 ) ;
#6114 = AXIS2_PLACEMENT_3D ( 'NONE', #2881, #24138, #18493 ) ;
#6115 = EDGE_LOOP ( 'NONE', ( #3703, #4356, #24721, #1853 ) ) ;
#6116 = EDGE_CURVE ( 'NONE', #25416, #2631, #8284, .T. ) ;
#6117 = LINE ( 'NONE', #13977, #22993 ) ;
#6118 = CARTESIAN_POINT ( 'NONE',  ( 42.81606138205700063, 16.19123852234703520, 80.30501292736995822 ) ) ;
#6119 = ORIENTED_EDGE ( 'NONE', *, *, #16404, .F. ) ;
#6120 = ADVANCED_FACE ( 'NONE', ( #19751 ), #25143, .F. ) ;
#6121 = CARTESIAN_POINT ( 'NONE',  ( 38.63098279924290068, -6.703840866421912459, 72.53360434286905445 ) ) ;
#6122 = ADVANCED_FACE ( 'NONE', ( #5592 ), #19883, .T. ) ;
#6123 = DIRECTION ( 'NONE',  ( 1.000000000000000000, 8.673617379884027583E-16, 0.000000000000000000 ) ) ;
#6124 = ORIENTED_EDGE ( 'NONE', *, *, #6702, .T. ) ;
#6125 = CARTESIAN_POINT ( 'NONE',  ( 45.81606138205697931, -30.45978664257862434, 43.58374455696579730 ) ) ;
#6126 = VERTEX_POINT ( 'NONE', #17701 ) ;
#6127 = ORIENTED_EDGE ( 'NONE', *, *, #13988, .F. ) ;
#6128 = DIRECTION ( 'NONE',  ( 1.000000000000000000, 0.000000000000000000, 0.000000000000000000 ) ) ;
#6129 = UNCERTAINTY_MEASURE_WITH_UNIT (LENGTH_MEASURE( 1.000000000000000082E-05 ), #12706, 'distance_accuracy_value', 'NONE');
#6130 = ADVANCED_BREP_SHAPE_REPRESENTATION ( '', ( #25224, #2000 ), #15364 ) ;
#6131 = CARTESIAN_POINT ( 'NONE',  ( 38.63098279924288647, -6.913682088886101695, 70.22690120949091863 ) ) ;
#6132 = CARTESIAN_POINT ( 'NONE',  ( 39.02742774030102879, -2.213682088886101518, 72.26730301774236409 ) ) ;
#6133 = ORIENTED_EDGE ( 'NONE', *, *, #23711, .T. ) ;
#6134 = ORIENTED_EDGE ( 'NONE', *, *, #9957, .F. ) ;
#6135 = CARTESIAN_POINT ( 'NONE',  ( 37.31606138205700063, 43.19123852234596939, 66.30501292736988717 ) ) ;
#6136 = FACE_OUTER_BOUND ( 'NONE', #13133, .T. ) ;
#6137 = LINE ( 'NONE', #24019, #24716 ) ;
#6138 = CARTESIAN_POINT ( 'NONE',  ( 39.82603832034400426, -19.30384086642190056, 70.35351908239857721 ) ) ;
#6139 = AXIS2_PLACEMENT_3D ( 'NONE', #24065, #14038, #10557 ) ;
#6140 = CYLINDRICAL_SURFACE ( 'NONE', #1317, 0.7500000000000006661 ) ;
#6141 = CARTESIAN_POINT ( 'NONE',  ( 33.81606138205700063, 15.19123852234700323, 70.30501292736995822 ) ) ;
#6142 = DIRECTION ( 'NONE',  ( 0.000000000000000000, -1.000000000000000000, 0.000000000000000000 ) ) ;
#6143 = ORIENTED_EDGE ( 'NONE', *, *, #15413, .T. ) ;
#6144 = AXIS2_PLACEMENT_3D ( 'NONE', #12895, #18555, #18805 ) ;
#6145 = VERTEX_POINT ( 'NONE', #15376 ) ;
#6146 = CIRCLE ( 'NONE', #7394, 10.50000000000000000 ) ;
#6147 = LINE ( 'NONE', #16180, #13301 ) ;
#6148 = CARTESIAN_POINT ( 'NONE',  ( 38.93415946300898867, -12.11368208888610631, 73.09843995877329803 ) ) ;
#6149 = EDGE_CURVE ( 'NONE', #6360, #4384, #31, .T. ) ;
#6150 = LINE ( 'NONE', #4473, #4021 ) ;
#6151 = CARTESIAN_POINT ( 'NONE',  ( 43.31606138205700063, -13.25716901376041967, 21.21736665487721041 ) ) ;
#6152 = AXIS2_PLACEMENT_3D ( 'NONE', #11733, #19432, #13523 ) ;
#6153 = CARTESIAN_POINT ( 'NONE',  ( 44.81606138205700063, -36.55876147765400930, 73.30501292737011454 ) ) ;
#6154 = FACE_BOUND ( 'NONE', #12545, .T. ) ;
#6155 = AXIS2_PLACEMENT_3D ( 'NONE', #9741, #25034, #17592 ) ;
#6156 = CARTESIAN_POINT ( 'NONE',  ( 30.81606138205700418, 34.87886987267149408, 66.30501292737000085 ) ) ;
#6157 = CARTESIAN_POINT ( 'NONE',  ( 44.71606138205695657, 0.5799492015812843793, -3.145019409304214530 ) ) ;
#6158 = ORIENTED_EDGE ( 'NONE', *, *, #10827, .T. ) ;
#6159 = CARTESIAN_POINT ( 'NONE',  ( 36.51582732573286449, -21.10256731895815463, 75.36702044841622694 ) ) ;
#6160 = ORIENTED_EDGE ( 'NONE', *, *, #22164, .F. ) ;
#6161 = ORIENTED_EDGE ( 'NONE', *, *, #4833, .F. ) ;
#6162 = CARTESIAN_POINT ( 'NONE',  ( 40.26954217208372455, -6.903840866421917966, 72.86986841596736042 ) ) ;
#6163 = ORIENTED_EDGE ( 'NONE', *, *, #23820, .F. ) ;
#6164 = LINE ( 'NONE', #15558, #2128 ) ;
#6165 = CARTESIAN_POINT ( 'NONE',  ( 37.69796330110504101, -9.113682088886100985, 69.66206559358663242 ) ) ;
#6166 = AXIS2_PLACEMENT_3D ( 'NONE', #8834, #3396, #11275 ) ;
#6167 = VERTEX_POINT ( 'NONE', #21301 ) ;
#6168 = DIRECTION ( 'NONE',  ( -1.123589211228918605E-15, 0.4425581086832399147, -0.8967398287344627850 ) ) ;
#6169 = CARTESIAN_POINT ( 'NONE',  ( 38.26194895904383486, -15.01368208888610134, 69.04448340153878405 ) ) ;
#6170 = EDGE_CURVE ( 'NONE', #14470, #20177, #5949, .T. ) ;
#6171 = VECTOR ( 'NONE', #19324, 1000.000000000000114 ) ;
#6172 =( BOUNDED_SURFACE ( )  B_SPLINE_SURFACE ( 3, 1, ( 
 ( #17042, #11373 ),
 ( #13551, #7757 ),
 ( #5438, #21539 ),
 ( #23199, #15349 ) ),
 .UNSPECIFIED., .F., .F., .T. ) 
 B_SPLINE_SURFACE_WITH_KNOTS ( ( 4, 4 ),
 ( 2, 2 ),
 ( 0.000000000000000000, 1.000000000000000000 ),
 ( 0.000000000000000000, 1.000000000000000000 ),
 .UNSPECIFIED. ) 
 GEOMETRIC_REPRESENTATION_ITEM ( )  RATIONAL_B_SPLINE_SURFACE ( (
 ( 1.000000000000000000, 1.000000000000000000),
 ( 0.8047378541243649375, 0.8047378541243649375),
 ( 0.8047378541243649375, 0.8047378541243649375),
 ( 1.000000000000000000, 1.000000000000000000) ) ) 
 REPRESENTATION_ITEM ( '' )  SURFACE ( )  );
#6173 = DIRECTION ( 'NONE',  ( 1.000000000000000000, 0.000000000000000000, 0.000000000000000000 ) ) ;
#6174 = EDGE_CURVE ( 'NONE', #24859, #17007, #3644, .T. ) ;
#6175 = LINE ( 'NONE', #7989, #16555 ) ;
#6176 = EDGE_CURVE ( 'NONE', #1075, #12192, #15393, .T. ) ;
#6177 = CIRCLE ( 'NONE', #11105, 1.249999999999998890 ) ;
#6178 = DIRECTION ( 'NONE',  ( 1.000000000000000000, 0.000000000000000000, 0.000000000000000000 ) ) ;
#6179 = FILL_AREA_STYLE_COLOUR ( '', #21977 ) ;
#6180 = DIRECTION ( 'NONE',  ( 0.000000000000000000, -1.000000000000000000, 2.999999999999999839E-15 ) ) ;
#6181 = PRODUCT_DEFINITION_SHAPE ( 'NONE', 'NONE',  #25500 ) ;
#6182 = DIRECTION ( 'NONE',  ( 0.000000000000000000, 0.6568589528324747517, -0.7540134720837718962 ) ) ;
#6183 = CARTESIAN_POINT ( 'NONE',  ( 36.31606138205698642, -8.139132291388525786, 32.47600601670134779 ) ) ;
#6184 = CARTESIAN_POINT ( 'NONE',  ( 37.12184278917507640, -23.51368208888609956, 71.43714994484032843 ) ) ;
#6185 = ORIENTED_EDGE ( 'NONE', *, *, #22647, .F. ) ;
#6186 = AXIS2_PLACEMENT_3D ( 'NONE', #23576, #21649, #11878 ) ;
#6187 = LINE ( 'NONE', #3991, #25483 ) ;
#6188 = ADVANCED_FACE ( 'NONE', ( #23480 ), #5844, .F. ) ;
#6189 = DIRECTION ( 'NONE',  ( 1.000000000000000000, 1.734723475976804876E-16, -1.734723475976814737E-16 ) ) ;
#6190 = ORIENTED_EDGE ( 'NONE', *, *, #13277, .T. ) ;
#6191 = ORIENTED_EDGE ( 'NONE', *, *, #18853, .F. ) ;
#6192 = UNCERTAINTY_MEASURE_WITH_UNIT (LENGTH_MEASURE( 1.000000000000000082E-05 ), #10911, 'distance_accuracy_value', 'NONE');
#6193 = CIRCLE ( 'NONE', #10736, 1.500000000000000222 ) ;
#6194 = CARTESIAN_POINT ( 'NONE',  ( 36.07789103942399578, -22.20384086642191690, 72.05058123536544201 ) ) ;
#6195 = CARTESIAN_POINT ( 'NONE',  ( 39.82603832034400426, -26.31368208888611093, 72.40698646996131060 ) ) ;
#6196 = DIRECTION ( 'NONE',  ( -1.000000000000000000, 0.000000000000000000, 0.000000000000000000 ) ) ;
#6197 = FACE_OUTER_BOUND ( 'NONE', #18252, .T. ) ;
#6198 = ORIENTED_EDGE ( 'NONE', *, *, #19626, .F. ) ;
#6199 = CARTESIAN_POINT ( 'NONE',  ( 39.89406713111731051, -5.936539503995411415, 82.77827728996761891 ) ) ;
#6200 = DIRECTION ( 'NONE',  ( 0.000000000000000000, 3.469446951953611033E-15, 1.000000000000000000 ) ) ;
#6201 = CARTESIAN_POINT ( 'NONE',  ( 40.26954217208372455, -0.9038408664219198529, 72.86986841596736042 ) ) ;
#6202 = DIRECTION ( 'NONE',  ( 0.000000000000000000, -1.000000000000000000, 2.999999999999999839E-15 ) ) ;
#6203 = CARTESIAN_POINT ( 'NONE',  ( 39.98359781491296161, -8.413682088886105248, 71.86517103874048473 ) ) ;
#6204 = CARTESIAN_POINT ( 'NONE',  ( 36.31606138205700063, -13.58280000135113674, 20.54174511886706256 ) ) ;
#6205 = CIRCLE ( 'NONE', #7438, 0.2999999999999938827 ) ;
#6206 = CARTESIAN_POINT ( 'NONE',  ( 40.14115730948191185, -26.51368208888610667, 71.32335560751960202 ) ) ;
#6207 = CIRCLE ( 'NONE', #21427, 1.000000000000000888 ) ;
#6208 = CARTESIAN_POINT ( 'NONE',  ( 35.31606138205700773, 8.104266321858618838, 55.82104096753806033 ) ) ;
#6209 = CARTESIAN_POINT ( 'NONE',  ( 38.93415946300897446, -3.503840866421906952, 69.66206559358664663 ) ) ;
#6210 = DIRECTION ( 'NONE',  ( -6.489379976170840313E-31, 1.000000000000000000, -3.491481338843135327E-15 ) ) ;
#6211 = CARTESIAN_POINT ( 'NONE',  ( 39.51027997493896748, -25.10384086642191193, 71.43714994484031422 ) ) ;
#6212 = CARTESIAN_POINT ( 'NONE',  ( 38.26194895904383486, -9.013682088886101340, 69.64448340153879258 ) ) ;
#6213 = FACE_OUTER_BOUND ( 'NONE', #10599, .T. ) ;
#6214 = ADVANCED_FACE ( 'NONE', ( #16378 ), #12291, .T. ) ;
#6215 = CARTESIAN_POINT ( 'NONE',  ( 36.49096545463212493, -14.10384086642191015, 71.32335560751961623 ) ) ;
#6216 = CARTESIAN_POINT ( 'NONE',  ( 44.31606138205700063, -21.26162886970023536, 44.16441745890789150 ) ) ;
#6217 = VECTOR ( 'NONE', #2633, 1000.000000000000227 ) ;
#6218 = CARTESIAN_POINT ( 'NONE',  ( 39.75915168707250302, -14.71368208888610063, 70.26145752964251301 ) ) ;
#6219 = ORIENTED_EDGE ( 'NONE', *, *, #11381, .F. ) ;
#6220 = CARTESIAN_POINT ( 'NONE',  ( 36.07789103942398867, -17.41368208888610525, 70.70992431699450265 ) ) ;
#6221 = ORIENTED_EDGE ( 'NONE', *, *, #7705, .T. ) ;
#6222 = DIRECTION ( 'NONE',  ( 3.540251991789399939E-16, 2.999999999999999839E-15, 1.000000000000000000 ) ) ;
#6223 = FACE_OUTER_BOUND ( 'NONE', #24949, .T. ) ;
#6224 = AXIS2_PLACEMENT_3D ( 'NONE', #3298, #14767, #22624 ) ;
#6225 = CARTESIAN_POINT ( 'NONE',  ( 37.25260217561390874, -20.00384086642191406, 70.97781676520601479 ) ) ;
#6226 = EDGE_LOOP ( 'NONE', ( #13860, #15124, #4034, #4045 ) ) ;
#6227 = ORIENTED_EDGE ( 'NONE', *, *, #18105, .F. ) ;
#6228 = CARTESIAN_POINT ( 'NONE',  ( 40.64099152588522657, 1.392818861812999964, 84.30501292737000085 ) ) ;
#6229 = LINE ( 'NONE', #10103, #20300 ) ;
#6230 = CARTESIAN_POINT ( 'NONE',  ( 40.55423172469004101, -21.20384086642191690, 70.70992431699450265 ) ) ;
#6231 = FACE_OUTER_BOUND ( 'NONE', #13717, .T. ) ;
#6232 = CARTESIAN_POINT ( 'NONE',  ( 38.93415946300897446, -24.11368208888610454, 73.09843995877328382 ) ) ;
#6233 = PRODUCT_DEFINITION_SHAPE ( 'NONE', 'NONE',  #20652 ) ;
#6234 = DIRECTION ( 'NONE',  ( -1.000000000000000000, -1.734723475976804876E-16, 1.734723475976814737E-16 ) ) ;
#6235 = VERTEX_POINT ( 'NONE', #20134 ) ;
#6236 = ORIENTED_EDGE ( 'NONE', *, *, #24117, .F. ) ;
#6237 = CARTESIAN_POINT ( 'NONE',  ( 33.31606138205700773, 7.283211578144648257, 66.04722806671131252 ) ) ;
#6238 = FACE_OUTER_BOUND ( 'NONE', #17631, .T. ) ;
#6239 = CARTESIAN_POINT ( 'NONE',  ( 39.29254315202757653, -22.80384086642191477, 72.81632618279321889 ) ) ;
#6240 = DIRECTION ( 'NONE',  ( 0.000000000000000000, -2.913263826201159484E-15, -1.000000000000000000 ) ) ;
#6241 = ORIENTED_EDGE ( 'NONE', *, *, #7493, .F. ) ;
#6242 = DIRECTION ( 'NONE',  ( 1.000000000000000000, 0.000000000000000000, -0.000000000000000000 ) ) ;
#6243 = ADVANCED_FACE ( 'NONE', ( #537 ), #18456, .F. ) ;
#6244 = CARTESIAN_POINT ( 'NONE',  ( 41.81606138205697221, -3.103162021984027241, -5.046558096268735305 ) ) ;
#6245 = CARTESIAN_POINT ( 'NONE',  ( 38.26194895904384197, 1.396159133578087186, 72.51602215082118619 ) ) ;
#6246 = DIRECTION ( 'NONE',  ( 0.3420484745865489673, -0.7716719862102489058, -0.5362137509718902795 ) ) ;
#6247 = ORIENTED_EDGE ( 'NONE', *, *, #7536, .T. ) ;
#6248 = FACE_BOUND ( 'NONE', #12703, .T. ) ;
#6249 = ORIENTED_EDGE ( 'NONE', *, *, #13341, .F. ) ;
#6250 = EDGE_LOOP ( 'NONE', ( #15505, #9557, #24312, #22938 ) ) ;
#6251 = DIRECTION ( 'NONE',  ( -1.000000000000000000, 1.115179377413661005E-30, 3.717264591378870232E-16 ) ) ;
#6252 = CYLINDRICAL_SURFACE ( 'NONE', #10051, 10.50000000000000000 ) ;
#6253 = CARTESIAN_POINT ( 'NONE',  ( 39.24876120206128860, -4.713682088886099741, 70.63227792289247020 ) ) ;
#6254 = CARTESIAN_POINT ( 'NONE',  ( 39.41296390513587511, -4.413682088886102584, 71.67976084211552745 ) ) ;
#6255 = EDGE_LOOP ( 'NONE', ( #17149, #780, #19183, #11557 ) ) ;
#6256 = ORIENTED_EDGE ( 'NONE', *, *, #14050, .T. ) ;
#6257 = DIRECTION ( 'NONE',  ( 0.000000000000000000, 0.1918498038142811835, -0.9814242980364923374 ) ) ;
#6258 = DIRECTION ( 'NONE',  ( -1.849283715844614456E-16, 0.8212051873014208914, 0.5706330172266919076 ) ) ;
#6259 = ORIENTED_EDGE ( 'NONE', *, *, #649, .F. ) ;
#6260 = DIRECTION ( 'NONE',  ( -1.327674326049719602E-15, 0.4425581086832399147, -0.8967398287344627850 ) ) ;
#6261 = VECTOR ( 'NONE', #20515, 1000.000000000000000 ) ;
#6262 = CARTESIAN_POINT ( 'NONE',  ( 36.87297107704149823, -9.903840866421901978, 70.26145752964255564 ) ) ;
#6263 = AXIS2_PLACEMENT_3D ( 'NONE', #4787, #20508, #25073 ) ;
#6264 = EDGE_CURVE ( 'NONE', #18120, #536, #8545, .T. ) ;
#6265 = EDGE_CURVE ( 'NONE', #11430, #1915, #6362, .T. ) ;
#6266 = LINE ( 'NONE', #24481, #6261 ) ;
#6267 = VECTOR ( 'NONE', #14892, 1000.000000000000227 ) ;
#6268 = DIRECTION ( 'NONE',  ( -1.000000000000000000, 0.000000000000000000, 0.000000000000000000 ) ) ;
#6269 = EDGE_CURVE ( 'NONE', #19362, #16440, #581, .T. ) ;
#6270 = VERTEX_POINT ( 'NONE', #22190 ) ;
#6271 = ORIENTED_EDGE ( 'NONE', *, *, #3529, .T. ) ;
#6272 = EDGE_CURVE ( 'NONE', #22152, #17202, #3883, .T. ) ;
#6273 = EDGE_CURVE ( 'NONE', #7938, #24390, #8290, .T. ) ;
#6274 = VERTEX_POINT ( 'NONE', #6731 ) ;
#6275 = CARTESIAN_POINT ( 'NONE',  ( 34.81606138205697221, -3.103162021984047669, -5.046558096268735305 ) ) ;
#6276 = CARTESIAN_POINT ( 'NONE',  ( 36.87297107704153376, -7.713682088886109511, 72.49904802271743165 ) ) ;
#6277 = DIRECTION ( 'NONE',  ( 1.000000000000000000, 1.817449160981365809E-30, -1.734723475976805122E-15 ) ) ;
#6278 = CARTESIAN_POINT ( 'NONE',  ( 35.64099152588523367, -1.357181138186998925, 88.30501292736998664 ) ) ;
#6279 = LINE ( 'NONE', #13881, #5320 ) ;
#6280 = DIRECTION ( 'NONE',  ( 1.000000000000000000, 0.000000000000000000, 0.000000000000000000 ) ) ;
#6281 = ADVANCED_FACE ( 'NONE', ( #10221 ), #17961, .F. ) ;
#6282 = EDGE_CURVE ( 'NONE', #16594, #16761, #23983, .T. ) ;
#6283 = VECTOR ( 'NONE', #23805, 1000.000000000000000 ) ;
#6284 = DIRECTION ( 'NONE',  ( 0.000000000000000000, -0.6568589528324746407, 0.7540134720837717852 ) ) ;
#6285 = DIRECTION ( 'NONE',  ( 1.000000000000000000, 2.952017753711455077E-15, 9.722472704681867976E-17 ) ) ;
#6286 = CIRCLE ( 'NONE', #7950, 0.2000000000000057288 ) ;
#6287 = FACE_OUTER_BOUND ( 'NONE', #19389, .T. ) ;
#6288 = ORIENTED_EDGE ( 'NONE', *, *, #22314, .T. ) ;
#6289 = ORIENTED_EDGE ( 'NONE', *, *, #16719, .T. ) ;
#6290 = DIRECTION ( 'NONE',  ( 0.000000000000000000, 0.6568589528324746407, -0.7540134720837717852 ) ) ;
#6291 = CARTESIAN_POINT ( 'NONE',  ( 40.55423172469004101, -7.203840866421916900, 70.70992431699450265 ) ) ;
#6292 = ORIENTED_EDGE ( 'NONE', *, *, #24317, .T. ) ;
#6293 = EDGE_CURVE ( 'NONE', #21203, #12220, #22317, .T. ) ;
#6294 = TOROIDAL_SURFACE ( 'NONE', #2553, 1.800000000000000044, 0.2000000000000000111 ) ;
#6295 = DIRECTION ( 'NONE',  ( 1.000000000000000000, 3.259265938791515726E-15, 1.279526567694519919E-16 ) ) ;
#6296 = CARTESIAN_POINT ( 'NONE',  ( 38.37017380507020192, -6.013682088886109334, 73.11602215082118050 ) ) ;
#6297 = ORIENTED_EDGE ( 'NONE', *, *, #1823, .F. ) ;
#6298 = CARTESIAN_POINT ( 'NONE',  ( 43.31606138205700063, 2.476587234117772596, 12.62587505415466538 ) ) ;
#6299 = AXIS2_PLACEMENT_3D ( 'NONE', #15920, #20265, #2602 ) ;
#6300 = CARTESIAN_POINT ( 'NONE',  ( 38.37017380507020192, -18.01368208888610667, 73.71602215082113219 ) ) ;
#6301 = CIRCLE ( 'NONE', #2576, 1.000000000000000888 ) ;
#6302 = EDGE_CURVE ( 'NONE', #8221, #23347, #10481, .T. ) ;
#6303 = DIRECTION ( 'NONE',  ( -1.000000000000000000, 0.000000000000000000, 0.000000000000000000 ) ) ;
#6304 = DIRECTION ( 'NONE',  ( 0.000000000000000000, -1.632680918566405215E-15, 1.000000000000000000 ) ) ;
#6305 = VECTOR ( 'NONE', #9192, 1000.000000000000000 ) ;
#6306 = ORIENTED_EDGE ( 'NONE', *, *, #11386, .F. ) ;
#6307 = CARTESIAN_POINT ( 'NONE',  ( 33.31606138205700773, -13.04008168869995288, 21.66778101221729713 ) ) ;
#6308 = CARTESIAN_POINT ( 'NONE',  ( 45.81606138205706458, -34.13844651005145181, 70.48338531520533934 ) ) ;
#6309 = VECTOR ( 'NONE', #20816, 1000.000000000000000 ) ;
#6310 = DIRECTION ( 'NONE',  ( 0.000000000000000000, 1.000000000000000000, -2.999999999999999839E-15 ) ) ;
#6311 = CARTESIAN_POINT ( 'NONE',  ( 32.81606138205700773, -35.41471100349711065, 71.53682070832086026 ) ) ;
#6312 = CARTESIAN_POINT ( 'NONE',  ( 39.51027997493896748, -22.51368208888609246, 71.32335560751960202 ) ) ;
#6313 = ORIENTED_EDGE ( 'NONE', *, *, #11618, .F. ) ;
#6314 = CARTESIAN_POINT ( 'NONE',  ( 39.64097644196145609, -21.72530145503456822, 75.31687860557157421 ) ) ;
#6315 = CARTESIAN_POINT ( 'NONE',  ( 45.81606138205700063, 36.92314894770294131, 81.17823623207321759 ) ) ;
#6316 = ORIENTED_EDGE ( 'NONE', *, *, #10381, .F. ) ;
#6317 = ORIENTED_EDGE ( 'NONE', *, *, #20599, .F. ) ;
#6318 = CARTESIAN_POINT ( 'NONE',  ( 39.64521430340305841, -20.80384086642191832, 73.30173637941818754 ) ) ;
#6319 = EDGE_CURVE ( 'NONE', #17478, #203, #2224, .T. ) ;
#6320 = AXIS2_PLACEMENT_3D ( 'NONE', #1014, #20863, #12891 ) ;
#6321 = CARTESIAN_POINT ( 'NONE',  ( 40.14115730948191185, -26.51368208888610667, 71.32335560751958781 ) ) ;
#6322 = EDGE_CURVE ( 'NONE', #12591, #194, #4303, .T. ) ;
#6323 = CARTESIAN_POINT ( 'NONE',  ( 36.31606138205700063, -26.06829118875199569, 75.80501292736998664 ) ) ;
#6324 = CARTESIAN_POINT ( 'NONE',  ( 33.31606138205700773, -22.22127907754180853, 85.30501292736998664 ) ) ;
#6325 = ORIENTED_EDGE ( 'NONE', *, *, #12714, .F. ) ;
#6326 = VECTOR ( 'NONE', #10111, 1000.000000000000000 ) ;
#6327 = CARTESIAN_POINT ( 'NONE',  ( 39.52152274622449113, -5.583621694698644333, 82.79804034237957922 ) ) ;
#6328 = DIRECTION ( 'NONE',  ( -1.000000000000000000, 0.000000000000000000, 0.000000000000000000 ) ) ;
#6329 = CARTESIAN_POINT ( 'NONE',  ( 39.64521430340305841, -4.803840866421917433, 73.30173637941818754 ) ) ;
#6330 = CARTESIAN_POINT ( 'NONE',  ( 43.31606138205700063, 3.536347952325769040, 64.10938348997790115 ) ) ;
#6331 = DIRECTION ( 'NONE',  ( 0.000000000000000000, -1.000000000000000000, 2.999999999999999839E-15 ) ) ;
#6332 = PRESENTATION_LAYER_ASSIGNMENT (  '', '', ( #17438 ) ) ;
#6333 = CARTESIAN_POINT ( 'NONE',  ( 36.49096545463212493, -5.513682088886105781, 71.43714994484035685 ) ) ;
#6334 = DIRECTION ( 'NONE',  ( -0.1733269559585509378, 0.000000000000000000, -0.9848643390529188135 ) ) ;
#6335 = CARTESIAN_POINT ( 'NONE',  ( 38.37017380507020192, -28.01368208888610667, 73.11602215082115208 ) ) ;
#6336 = CIRCLE ( 'NONE', #2201, 2.000000000000001776 ) ;
#6337 = CARTESIAN_POINT ( 'NONE',  ( 40.31606138205700773, -31.05876147765400574, 73.55501292737010033 ) ) ;
#6338 = AXIS2_PLACEMENT_3D ( 'NONE', #11343, #15183, #3336 ) ;
#6339 = LINE ( 'NONE', #2800, #7744 ) ;
#6340 = CONTEXT_DEPENDENT_SHAPE_REPRESENTATION ( #7341, #1261 ) ;
#6341 = CARTESIAN_POINT ( 'NONE',  ( 40.31606138205700773, -7.204193249396275256, 83.11277699141410835 ) ) ;
#6342 = CARTESIAN_POINT ( 'NONE',  ( 38.26194895904384197, -28.60384086642191193, 72.51602215082114355 ) ) ;
#6343 = CARTESIAN_POINT ( 'NONE',  ( 36.87297107704152666, -13.71368208888610773, 72.49904802271740323 ) ) ;
#6344 = DIRECTION ( 'NONE',  ( 1.000000000000000000, 2.870367030604242092E-15, -6.397632838472598363E-17 ) ) ;
#6345 = ADVANCED_FACE ( 'NONE', ( #2472 ), #10346, .F. ) ;
#6346 = CARTESIAN_POINT ( 'NONE',  ( 39.95015449827720744, -9.003840866421912281, 71.96809898377888715 ) ) ;
#6347 = LINE ( 'NONE', #6090, #22900 ) ;
#6348 = ADVANCED_FACE ( 'NONE', ( #8162 ), #2717, .T. ) ;
#6349 = PRESENTATION_LAYER_ASSIGNMENT (  '', '', ( #19923 ) ) ;
#6350 = EDGE_CURVE ( 'NONE', #9234, #24670, #24355, .T. ) ;
#6351 = CARTESIAN_POINT ( 'NONE',  ( 38.82593461698262871, -12.91368208888610347, 69.62690120949091011 ) ) ;
#6352 = ORIENTED_EDGE ( 'NONE', *, *, #6726, .T. ) ;
#6353 = CARTESIAN_POINT ( 'NONE',  ( 39.64521430340304420, -16.81368208888610383, 69.45876917294175712 ) ) ;
#6354 = ORIENTED_EDGE ( 'NONE', *, *, #2001, .T. ) ;
#6355 = PLANE ( 'NONE',  #8657 ) ;
#6356 = VECTOR ( 'NONE', #8042, 1000.000000000000000 ) ;
#6357 = CIRCLE ( 'NONE', #20752, 0.7499999999999983347 ) ;
#6358 = PLANE ( 'NONE',  #8362 ) ;
#6359 = CARTESIAN_POINT ( 'NONE',  ( 37.69225076346193504, -19.80384086642191477, 70.42958956619168021 ) ) ;
#6360 = VERTEX_POINT ( 'NONE', #6228 ) ;
#6361 = ORIENTED_EDGE ( 'NONE', *, *, #11620, .T. ) ;
#6362 = LINE ( 'NONE', #14335, #11719 ) ;
#6363 = DIRECTION ( 'NONE',  ( -3.299742535180970203E-16, 0.3299742535180970049, -0.9439899321577400748 ) ) ;
#6364 = CARTESIAN_POINT ( 'NONE',  ( 36.36258059203030513, -23.90384086642191619, 69.89063713639258424 ) ) ;
#6365 = DIRECTION ( 'NONE',  ( -1.000000000000000000, 0.000000000000000000, 0.000000000000000000 ) ) ;
#6366 = CARTESIAN_POINT ( 'NONE',  ( 39.12911128074873801, 1.886317911113891244, 73.69843995877330656 ) ) ;
#6367 = EDGE_CURVE ( 'NONE', #13507, #6369, #1435, .T. ) ;
#6368 = PLANE ( 'NONE',  #6912 ) ;
#6369 = VERTEX_POINT ( 'NONE', #22568 ) ;
#6370 = CARTESIAN_POINT ( 'NONE',  ( 33.72038411900482657, 3.276404855341859879, 6.354292672467103387 ) ) ;
#6371 = PRODUCT_DEFINITION_FORMATION_WITH_SPECIFIED_SOURCE ( 'ANY', '', #23697, .NOT_KNOWN. ) ;
#6372 = CYLINDRICAL_SURFACE ( 'NONE', #22099, 2.500000000000002220 ) ;
#6373 = CARTESIAN_POINT ( 'NONE',  ( 37.69796330110505522, -14.50384086642191583, 73.09843995877329803 ) ) ;
#6374 = CARTESIAN_POINT ( 'NONE',  ( 44.71606138205697079, -3.195232061939673240, -6.457771442202879797 ) ) ;
#6375 = ORIENTED_EDGE ( 'NONE', *, *, #9687, .T. ) ;
#6376 = DIRECTION ( 'NONE',  ( -3.717264591378870232E-16, -2.999999999999999839E-15, -1.000000000000000000 ) ) ;
#6377 = CIRCLE ( 'NONE', #3067, 0.7500000000000006661 ) ;
#6378 = CARTESIAN_POINT ( 'NONE',  ( 46.81606138205701484, -19.40517585842700043, 23.66972737280834238 ) ) ;
#6379 = CARTESIAN_POINT ( 'NONE',  ( 38.37017380507018771, 0.3961591335780896284, 70.24448340153880110 ) ) ;
#6380 = LINE ( 'NONE', #14356, #23430 ) ;
#6381 = ORIENTED_EDGE ( 'NONE', *, *, #1316, .F. ) ;
#6382 = CARTESIAN_POINT ( 'NONE',  ( 39.95015449827720744, -28.61368208888610454, 70.79240656858104330 ) ) ;
#6383 = ORIENTED_EDGE ( 'NONE', *, *, #13, .F. ) ;
#6384 = ORIENTED_EDGE ( 'NONE', *, *, #2795, .T. ) ;
#6385 = CARTESIAN_POINT ( 'NONE',  ( 36.31606138205700063, 43.19123852234596939, 66.30501292736988717 ) ) ;
#6386 = FACE_OUTER_BOUND ( 'NONE', #10307, .T. ) ;
#6387 = CARTESIAN_POINT ( 'NONE',  ( 39.37952058850012804, -4.613682088886100985, 70.97781676520601479 ) ) ;
#6388 = CARTESIAN_POINT ( 'NONE',  ( 37.25260217561390874, -7.613682088886100985, 71.78268878715394408 ) ) ;
#6389 = ORIENTED_EDGE ( 'NONE', *, *, #3205, .T. ) ;
#6390 = EDGE_LOOP ( 'NONE', ( #7960, #14174, #20408, #21400 ) ) ;
#6391 = DIRECTION ( 'NONE',  ( -1.000000000000000000, -3.965082230804126670E-15, 0.000000000000000000 ) ) ;
#6392 = LINE ( 'NONE', #4458, #21908 ) ;
#6393 = ORIENTED_EDGE ( 'NONE', *, *, #3919, .T. ) ;
#6394 = CARTESIAN_POINT ( 'NONE',  ( 32.81606138205700773, 2.476587234117772596, 12.62587505415466538 ) ) ;
#6395 = CARTESIAN_POINT ( 'NONE',  ( 39.29254315202757653, -12.80384086642191299, 72.81632618279321889 ) ) ;
#6396 = AXIS2_PLACEMENT_3D ( 'NONE', #19849, #24197, #2310 ) ;
#6397 = AXIS2_PLACEMENT_3D ( 'NONE', #21913, #8519, #18058 ) ;
#6398 = DIRECTION ( 'NONE',  ( 1.000000000000000000, 4.087515222582816494E-17, 3.560839518387611236E-17 ) ) ;
#6399 = ADVANCED_FACE ( 'NONE', ( #24866 ), #3233, .T. ) ;
#6400 = FACE_OUTER_BOUND ( 'NONE', #10407, .T. ) ;
#6401 = ORIENTED_EDGE ( 'NONE', *, *, #9133, .F. ) ;
#6402 = EDGE_LOOP ( 'NONE', ( #24125, #535, #17993, #5136 ) ) ;
#6403 = ORIENTED_EDGE ( 'NONE', *, *, #7196, .F. ) ;
#6404 = PLANE ( 'NONE',  #7545 ) ;
#6405 = CARTESIAN_POINT ( 'NONE',  ( 39.82603832034401847, -8.313682088886109156, 72.40698646996133903 ) ) ;
#6406 = ORIENTED_EDGE ( 'NONE', *, *, #22491, .F. ) ;
#6407 = DIRECTION ( 'NONE',  ( 0.000000000000000000, 2.999999999999999839E-15, 1.000000000000000000 ) ) ;
#6408 = DIRECTION ( 'NONE',  ( -1.000000000000000000, -1.000000000000000078E-15, 0.000000000000000000 ) ) ;
#6409 = CARTESIAN_POINT ( 'NONE',  ( 33.31606138205700773, -5.204193249396277032, 83.30501292736992980 ) ) ;
#6410 = DIRECTION ( 'NONE',  ( 1.000000000000000000, 8.911169920151748851E-16, 3.114923731923493702E-16 ) ) ;
#6411 = CARTESIAN_POINT ( 'NONE',  ( 31.81606138205700418, -38.55876147765410167, 72.21586839016146087 ) ) ;
#6412 = FACE_OUTER_BOUND ( 'NONE', #14357, .T. ) ;
#6413 = EDGE_CURVE ( 'NONE', #23317, #13033, #20898, .T. ) ;
#6414 = EDGE_CURVE ( 'NONE', #12560, #21390, #21192, .T. ) ;
#6415 = DIRECTION ( 'NONE',  ( -1.445602896647339903E-16, 1.000000000000000000, -2.999999999999999839E-15 ) ) ;
#6416 = EDGE_LOOP ( 'NONE', ( #15821, #22360, #20683, #13474 ) ) ;
#6417 = EDGE_CURVE ( 'NONE', #3872, #5682, #24603, .T. ) ;
#6418 = EDGE_LOOP ( 'NONE', ( #15073, #3149, #24540, #6768 ) ) ;
#6419 = DIRECTION ( 'NONE',  ( -1.000000000000000000, 0.000000000000000000, -0.000000000000000000 ) ) ;
#6420 = CARTESIAN_POINT ( 'NONE',  ( 38.26194895904384197, -2.603840866421920364, 73.71602215082116061 ) ) ;
#6421 = EDGE_CURVE ( 'NONE', #17758, #2946, #18966, .T. ) ;
#6422 = VERTEX_POINT ( 'NONE', #8805 ) ;
#6423 = DIRECTION ( 'NONE',  ( -0.000000000000000000, -0.4425581086832399702, 0.8967398287344626739 ) ) ;
#6424 = CARTESIAN_POINT ( 'NONE',  ( 39.29254315202756231, -6.813682088886101162, 69.94417936956673998 ) ) ;
#6425 = CARTESIAN_POINT ( 'NONE',  ( 33.31606138205700773, -22.22127907754180853, 85.30501292736998664 ) ) ;
#6426 = ADVANCED_FACE ( 'NONE', ( #16645, #17037, #14836 ), #5187, .F. ) ;
#6427 = CARTESIAN_POINT ( 'NONE',  ( 39.12911128074873801, -14.11368208888610987, 73.69843995877327814 ) ) ;
#6428 = CARTESIAN_POINT ( 'NONE',  ( 40.31606138205700773, -29.30876147765401640, 69.30501292737010033 ) ) ;
#6429 = CARTESIAN_POINT ( 'NONE',  ( 32.99554091088185714, 3.410282305729706032, 6.167518378462459872 ) ) ;
#6430 = DIRECTION ( 'NONE',  ( 1.000000000000000000, -1.582848796673007376E-16, -1.099878323500689822E-16 ) ) ;
#6431 =( NAMED_UNIT ( * ) SI_UNIT ( $, .STERADIAN. ) SOLID_ANGLE_UNIT ( ) );
#6432 = DIRECTION ( 'NONE',  ( 0.000000000000000000, -0.5706330172266920187, 0.8212051873014210024 ) ) ;
#6433 = DIRECTION ( 'NONE',  ( 0.000000000000000000, 1.000000000000000000, -2.921639538487253867E-15 ) ) ;
#6434 = CARTESIAN_POINT ( 'NONE',  ( 40.31606138205700773, -26.06829118875199569, 75.80501292736998664 ) ) ;
#6435 = CARTESIAN_POINT ( 'NONE',  ( 39.02742774030102879, -24.21368208888609885, 72.26730301774232146 ) ) ;
#6436 = VERTEX_POINT ( 'NONE', #12796 ) ;
#6437 = CARTESIAN_POINT ( 'NONE',  ( 38.83707137437546919, -22.15666622595546187, 75.30518859485255234 ) ) ;
#6438 = FACE_OUTER_BOUND ( 'NONE', #19775, .T. ) ;
#6439 = ORIENTED_EDGE ( 'NONE', *, *, #10957, .F. ) ;
#6440 = ORIENTED_EDGE ( 'NONE', *, *, #5750, .T. ) ;
#6441 = CARTESIAN_POINT ( 'NONE',  ( 36.98690846071097127, -23.80384086642191477, 69.45876917294174291 ) ) ;
#6442 = EDGE_CURVE ( 'NONE', #6126, #5370, #23213, .T. ) ;
#6443 = EDGE_CURVE ( 'NONE', #14979, #22793, #15091, .T. ) ;
#6444 = CARTESIAN_POINT ( 'NONE',  ( 40.26954217208371034, 1.286317911113898260, 69.89063713639259845 ) ) ;
#6445 = CARTESIAN_POINT ( 'NONE',  ( 45.81606138205707168, -36.31746077171914067, 73.86860304758450013 ) ) ;
#6446 = DIRECTION ( 'NONE',  ( 2.727049986597864201E-15, -0.7516416929448760387, -0.6595716529892418079 ) ) ;
#6447 = DIRECTION ( 'NONE',  ( 1.000000000000000000, 0.000000000000000000, 0.000000000000000000 ) ) ;
#6448 = ORIENTED_EDGE ( 'NONE', *, *, #477, .T. ) ;
#6449 = DIRECTION ( 'NONE',  ( 0.000000000000000000, 0.9038432971286278761, 0.4278636397681519488 ) ) ;
#6450 = DIRECTION ( 'NONE',  ( -1.734723475976814737E-16, 1.000000000000000000, -3.491481338843135327E-15 ) ) ;
#6451 = CARTESIAN_POINT ( 'NONE',  ( 39.02088643472237806, -4.703840866421917788, 73.73360434286902887 ) ) ;
#6452 = DIRECTION ( 'NONE',  ( 0.000000000000000000, 0.8212051873014223347, 0.5706330172266899092 ) ) ;
#6453 = DIRECTION ( 'NONE',  ( -1.000000000000000000, 0.000000000000000000, 0.000000000000000000 ) ) ;
#6454 = CARTESIAN_POINT ( 'NONE',  ( 39.95015449827720744, -8.613682088886104538, 70.79240656858107172 ) ) ;
#6455 = CARTESIAN_POINT ( 'NONE',  ( 35.81606138205700063, 9.191238522346999673, 69.30501292736997243 ) ) ;
#6456 = CARTESIAN_POINT ( 'NONE',  ( 38.26194895904383486, -27.01368208888610312, 69.64448340153876416 ) ) ;
#6457 = DIRECTION ( 'NONE',  ( 1.000000000000000000, 0.000000000000000000, 0.000000000000000000 ) ) ;
#6458 = ADVANCED_FACE ( 'NONE', ( #5310 ), #10980, .F. ) ;
#6459 = DIRECTION ( 'NONE',  ( -3.717264591378870232E-16, -3.325260651745651169E-15, -1.000000000000000000 ) ) ;
#6460 = CARTESIAN_POINT ( 'NONE',  ( 37.89291511884479036, -28.50384086642191406, 72.49843995877328950 ) ) ;
#6461 = CARTESIAN_POINT ( 'NONE',  ( 36.80608444377001121, -15.31368208888610383, 70.35351908239857721 ) ) ;
#6462 = ORIENTED_EDGE ( 'NONE', *, *, #2155, .T. ) ;
#6463 = CYLINDRICAL_SURFACE ( 'NONE', #22590, 1.499999999999999778 ) ;
#6464 = AXIS2_PLACEMENT_3D ( 'NONE', #9572, #25251, #19726 ) ;
#6465 = VECTOR ( 'NONE', #2510, 1000.000000000000000 ) ;
#6466 = CARTESIAN_POINT ( 'NONE',  ( 39.98359781491296161, -11.20384086642191335, 70.89533451361947414 ) ) ;
#6467 = CARTESIAN_POINT ( 'NONE',  ( 33.40064408022072939, 41.67000142393845152, 79.37823623207322044 ) ) ;
#6468 = TOROIDAL_SURFACE ( 'NONE', #9357, 0.2314957320545545372, 0.5000000000000000000 ) ;
#6469 = CARTESIAN_POINT ( 'NONE',  ( 37.80618814713140097, -3.913682088886108801, 73.13360434286904876 ) ) ;
#6470 = ORIENTED_EDGE ( 'NONE', *, *, #8946, .T. ) ;
#6471 = CARTESIAN_POINT ( 'NONE',  ( 36.29569395875879678, -17.31368208888610383, 69.98269868914867686 ) ) ;
#6472 = VERTEX_POINT ( 'NONE', #7368 ) ;
#6473 = CARTESIAN_POINT ( 'NONE',  ( 43.06606138205700063, 41.44123852234599781, 74.30501292736987295 ) ) ;
#6474 = FACE_OUTER_BOUND ( 'NONE', #24445, .T. ) ;
#6475 = CARTESIAN_POINT ( 'NONE',  ( 37.25260217561390874, -18.00384086642191050, 70.97781676520601479 ) ) ;
#6476 = ORIENTED_EDGE ( 'NONE', *, *, #3571, .T. ) ;
#6477 = EDGE_LOOP ( 'NONE', ( #9815, #4058, #16252, #9239 ) ) ;
#6478 = CARTESIAN_POINT ( 'NONE',  ( 45.81606138205700063, 34.87886987267150118, 78.19668729537065133 ) ) ;
#6479 = CARTESIAN_POINT ( 'NONE',  ( 31.81606138205700418, -34.55876147765403061, 66.30501292737011454 ) ) ;
#6480 = CARTESIAN_POINT ( 'NONE',  ( 36.11133435605973574, -24.00384086642191761, 70.60699637195608602 ) ) ;
#6481 = LINE ( 'NONE', #2349, #18689 ) ;
#6482 = CARTESIAN_POINT ( 'NONE',  ( 39.98359781491296161, -24.41368208888610525, 71.86517103874045631 ) ) ;
#6483 = DIRECTION ( 'NONE',  ( -1.000000000000000000, -1.734723475976804876E-16, 1.734723475976814737E-16 ) ) ;
#6484 = CLOSED_SHELL ( 'NONE', ( #5560, #22262, #2935, #6997, #12277, #17151, #6348, #6243, #15984, #1584, #304, #4257, #18158, #14414, #20905, #5282, #23601, #9105, #13685, #8522, #11854, #3700, #8361, #4577, #14886, #18544, #20285, #13737, #14801, #16982, #11895, #6742, #6345, #20139, #8486, #8066, #24514, #428, #6716, #24495, #9573, #17197, #646, #15537, #14220, #14340, #9553, #23026, #11476, #6089, #17433, #24524, #13589, #20845, #11320, #13557, #18022, #17114, #22463, #11061, #12151, #21097, #16486, #11432, #22068, #7044, #15812, #4196, #17617, #11970, #24964, #17144, #7322, #12867, #11058, #4690, #1857, #23231, #18628, #11626, #12259, #13559, #25140, #19548, #15021, #17473, #22393, #23868, #21353, #15988, #21148, #1413, #13129, #24649, #6557, #5013, #20812, #10847, #10278, #1872, #9730, #8343, #5717, #3575, #8432, #10988, #11628, #8875, #2318, #15248, #14754, #5494, #767, #12141, #21849, #9501, #21047, #14512, #9048, #1367, #23647, #14342, #8775, #375, #7691, #2418 ) ) ;
#6485 = ADVANCED_FACE ( 'NONE', ( #21027 ), #23068, .F. ) ;
#6486 = EDGE_LOOP ( 'NONE', ( #12335, #2281, #24714, #16092 ) ) ;
#6487 = ADVANCED_FACE ( 'NONE', ( #20512 ), #18831, .F. ) ;
#6488 = AXIS2_PLACEMENT_3D ( 'NONE', #22704, #18977, #10746 ) ;
#6489 = AXIS2_PLACEMENT_3D ( 'NONE', #1497, #11192, #3318 ) ;
#6490 = CARTESIAN_POINT ( 'NONE',  ( 43.06606138205700063, 41.44123852234599070, 73.55501292736987295 ) ) ;
#6491 = DIRECTION ( 'NONE',  ( 0.000000000000000000, 3.469446951953613400E-15, 1.000000000000000000 ) ) ;
#6492 = CARTESIAN_POINT ( 'NONE',  ( 38.26194895904384907, -12.60384086642191548, 73.11602215082116629 ) ) ;
#6493 = FACE_OUTER_BOUND ( 'NONE', #11204, .T. ) ;
#6494 = CARTESIAN_POINT ( 'NONE',  ( 32.81606138205700773, 41.44123852234599070, 73.55501292736987295 ) ) ;
#6495 = LINE ( 'NONE', #6751, #2055 ) ;
#6496 = CARTESIAN_POINT ( 'NONE',  ( 37.31647492878124694, -0.3038408664219096056, 72.03616607671141026 ) ) ;
#6497 = CARTESIAN_POINT ( 'NONE',  ( 43.81606138205700063, 44.92314894770294131, 81.17823623207320338 ) ) ;
#6498 = VERTEX_POINT ( 'NONE', #10733 ) ;
#6499 = ADVANCED_FACE ( 'NONE', ( #18578 ), #915, .T. ) ;
#6500 = CARTESIAN_POINT ( 'NONE',  ( 32.31606138205700063, -20.55619265724211076, 44.11584019928223910 ) ) ;
#6501 = ORIENTED_EDGE ( 'NONE', *, *, #5814, .T. ) ;
#6502 = VERTEX_POINT ( 'NONE', #6850 ) ;
#6503 = AXIS2_PLACEMENT_3D ( 'NONE', #6028, #14143, #8471 ) ;
#6504 = DIRECTION ( 'NONE',  ( 0.000000000000000000, 0.000000000000000000, 1.000000000000000000 ) ) ;
#6505 = DIRECTION ( 'NONE',  ( 0.000000000000000000, -0.7540134720837717852, -0.6568589528324746407 ) ) ;
#6506 = CARTESIAN_POINT ( 'NONE',  ( 38.00113996487114321, -3.913682088886100807, 72.53360434286905445 ) ) ;
#6507 = VECTOR ( 'NONE', #17711, 1000.000000000000000 ) ;
#6508 = CARTESIAN_POINT ( 'NONE',  ( 38.63098279924288647, -2.913682088886100363, 70.22690120949091863 ) ) ;
#6509 = EDGE_LOOP ( 'NONE', ( #11407, #17313 ) ) ;
#6510 = ORIENTED_EDGE ( 'NONE', *, *, #18197, .F. ) ;
#6511 = CYLINDRICAL_SURFACE ( 'NONE', #7452, 3.000000000000002665 ) ;
#6512 = DIRECTION ( 'NONE',  ( -1.000000000000000000, -1.000000000000000078E-15, 0.000000000000000000 ) ) ;
#6513 = FILL_AREA_STYLE ('',( #9096 ) ) ;
#6514 = CARTESIAN_POINT ( 'NONE',  ( 38.26194895904384907, -8.603840866421915479, 73.11602215082118050 ) ) ;
#6515 = APPLICATION_CONTEXT ( 'automotive_design' ) ;
#6516 = LINE ( 'NONE', #14625, #14976 ) ;
#6517 = LINE ( 'NONE', #16422, #18384 ) ;
#6518 = ORIENTED_EDGE ( 'NONE', *, *, #16824, .F. ) ;
#6519 = ORIENTED_EDGE ( 'NONE', *, *, #21800, .T. ) ;
#6520 = ORIENTED_EDGE ( 'NONE', *, *, #7973, .F. ) ;
#6521 = CARTESIAN_POINT ( 'NONE',  ( 41.31606138205700063, 1.207247317117632335, 63.73818242441765847 ) ) ;
#6522 = CARTESIAN_POINT ( 'NONE',  ( 36.87297107704153376, -5.713682088886106847, 72.49904802271743165 ) ) ;
#6523 = CARTESIAN_POINT ( 'NONE',  ( 40.05245289102396100, -29.10876147765230115, 71.40796565871902146 ) ) ;
#6524 = LINE ( 'NONE', #6278, #23126 ) ;
#6525 = CIRCLE ( 'NONE', #2395, 4.000000000000000000 ) ;
#6526 = CARTESIAN_POINT ( 'NONE',  ( 40.11557105022964720, -29.10876147765400646, 71.37118765889773897 ) ) ;
#6527 = VECTOR ( 'NONE', #2287, 1000.000000000000000 ) ;
#6528 = DIRECTION ( 'NONE',  ( 1.000000000000000275E-15, -0.9439899321577400748, -0.3299742535180970049 ) ) ;
#6529 = DIRECTION ( 'NONE',  ( 1.327674326049701655E-15, -0.4425581086832336419, 0.8967398287344658936 ) ) ;
#6530 = EDGE_CURVE ( 'NONE', #12188, #21184, #14706, .T. ) ;
#6531 = CARTESIAN_POINT ( 'NONE',  ( 43.23147868389327897, 41.67000142393845152, 79.37823623207322044 ) ) ;
#6532 = ORIENTED_EDGE ( 'NONE', *, *, #8385, .T. ) ;
#6533 = ORIENTED_EDGE ( 'NONE', *, *, #446, .F. ) ;
#6534 = FACE_OUTER_BOUND ( 'NONE', #13113, .T. ) ;
#6535 = CARTESIAN_POINT ( 'NONE',  ( 40.52078840805429394, -1.003840866421915612, 72.15350918040385864 ) ) ;
#6536 = CIRCLE ( 'NONE', #2801, 10.00000000000000000 ) ;
#6537 = CARTESIAN_POINT ( 'NONE',  ( 39.02742774030102879, -22.21368208888610241, 72.26730301774234988 ) ) ;
#6538 = ORIENTED_EDGE ( 'NONE', *, *, #21591, .T. ) ;
#6539 = ORIENTED_EDGE ( 'NONE', *, *, #24117, .T. ) ;
#6540 = DIRECTION ( 'NONE',  ( -1.000000000000000000, -3.091505625455828697E-15, -4.515976121274772923E-17 ) ) ;
#6541 = CARTESIAN_POINT ( 'NONE',  ( 36.80608444377001121, -5.313682088886100274, 70.35351908239860563 ) ) ;
#6542 = CARTESIAN_POINT ( 'NONE',  ( 36.68196826583682935, -28.00384086642191050, 70.79240656858105751 ) ) ;
#6543 = VECTOR ( 'NONE', #4808, 1000.000000000000000 ) ;
#6544 = DIRECTION ( 'NONE',  ( 1.000000000000000000, 0.000000000000000000, 0.000000000000000000 ) ) ;
#6545 = CARTESIAN_POINT ( 'NONE',  ( 36.07789103942398867, -11.41368208888610525, 70.70992431699450265 ) ) ;
#6546 = AXIS2_PLACEMENT_3D ( 'NONE', #21991, #8088, #10272 ) ;
#6547 = CARTESIAN_POINT ( 'NONE',  ( 31.81606138205700418, 18.19123852234599426, 73.05501292736995822 ) ) ;
#6548 = DIRECTION ( 'NONE',  ( 0.000000000000000000, 0.8212051873014252212, 0.5706330172266858014 ) ) ;
#6549 = DIRECTION ( 'NONE',  ( 1.000000000000000000, 2.168404344971010101E-16, -1.734723475976814737E-16 ) ) ;
#6550 = CARTESIAN_POINT ( 'NONE',  ( 43.24580177837434292, 3.721690752961227755, 6.335617458560805382 ) ) ;
#6551 = VECTOR ( 'NONE', #8113, 1000.000000000000000 ) ;
#6552 = CARTESIAN_POINT ( 'NONE',  ( 43.24580177837434292, 3.721690752961224202, 6.335617458560805382 ) ) ;
#6553 = CARTESIAN_POINT ( 'NONE',  ( 36.31606138205700063, -22.22127907754180853, 85.30501292736998664 ) ) ;
#6554 = VECTOR ( 'NONE', #9958, 1000.000000000000000 ) ;
#6555 = EDGE_LOOP ( 'NONE', ( #16737, #24347, #19049, #22315 ) ) ;
#6556 = CARTESIAN_POINT ( 'NONE',  ( 43.31606138205700063, -12.76023008545320181, 21.53290024082827969 ) ) ;
#6557 = ADVANCED_FACE ( 'NONE', ( #4924 ), #10860, .F. ) ;
#6558 = CARTESIAN_POINT ( 'NONE',  ( 44.81606138205700063, 40.39281886181299797, 82.55501292736983032 ) ) ;
#6559 = ORIENTED_EDGE ( 'NONE', *, *, #11868, .T. ) ;
#6560 = VERTEX_POINT ( 'NONE', #19338 ) ;
#6561 = CARTESIAN_POINT ( 'NONE',  ( 36.36258059203030513, -25.90384086642191264, 69.89063713639258424 ) ) ;
#6562 = AXIS2_PLACEMENT_3D ( 'NONE', #10788, #12984, #977 ) ;
#6563 = CARTESIAN_POINT ( 'NONE',  ( 36.68196826583682935, -25.61368208888610454, 71.96809898377887293 ) ) ;
#6564 = CARTESIAN_POINT ( 'NONE',  ( 43.06606138205700063, 43.19123852234599070, 73.55501292736987295 ) ) ;
#6565 = VECTOR ( 'NONE', #6284, 1000.000000000000227 ) ;
#6566 = CARTESIAN_POINT ( 'NONE',  ( 40.31606138205700773, -18.80550481115971095, 25.27912300651437150 ) ) ;
#6567 = ORIENTED_EDGE ( 'NONE', *, *, #19313, .F. ) ;
#6568 = DIRECTION ( 'NONE',  ( 2.792262043613788535E-15, -0.8967398287344627850, -0.4425581086832399147 ) ) ;
#6569 = PLANE ( 'NONE',  #8382 ) ;
#6570 = CARTESIAN_POINT ( 'NONE',  ( 40.26954217208372455, -2.903840866421918410, 72.86986841596736042 ) ) ;
#6571 = EDGE_CURVE ( 'NONE', #5342, #3483, #1671, .T. ) ;
#6572 = DIRECTION ( 'NONE',  ( 0.000000000000000000, 1.000000000000000000, 0.000000000000000000 ) ) ;
#6573 = LINE ( 'NONE', #21789, #9950 ) ;
#6574 = CARTESIAN_POINT ( 'NONE',  ( 36.80608444377001121, -7.313682088886100274, 70.35351908239860563 ) ) ;
#6575 = CARTESIAN_POINT ( 'NONE',  ( 43.81606138205700063, -27.17722769842920272, 59.42551550655435477 ) ) ;
#6576 = EDGE_CURVE ( 'NONE', #6034, #10160, #13422, .T. ) ;
#6577 = CARTESIAN_POINT ( 'NONE',  ( 39.29254315202756231, -22.81368208888610027, 69.94417936956672577 ) ) ;
#6578 = ADVANCED_FACE ( 'NONE', ( #9565, #21532 ), #9816, .T. ) ;
#6579 = ADVANCED_FACE ( 'NONE', ( #1548 ), #15851, .F. ) ;
#6580 = CIRCLE ( 'NONE', #9890, 2.000000000000000000 ) ;
#6581 = EDGE_CURVE ( 'NONE', #15661, #4935, #15731, .T. ) ;
#6582 = CARTESIAN_POINT ( 'NONE',  ( 43.31606138205700063, -4.357181138186123626, 83.30501292736992980 ) ) ;
#6583 = CARTESIAN_POINT ( 'NONE',  ( 43.81606138205700063, -40.62725863591898445, 68.52362519861142687 ) ) ;
#6584 = CIRCLE ( 'NONE', #21391, 0.5000000000000008882 ) ;
#6585 = CARTESIAN_POINT ( 'NONE',  ( 39.51027997493896748, -27.10384086642191903, 71.43714994484031422 ) ) ;
#6586 = CARTESIAN_POINT ( 'NONE',  ( 36.64852494920107517, -11.41368208888610525, 70.89533451361947414 ) ) ;
#6587 = DIRECTION ( 'NONE',  ( -2.048868001712896742E-15, 0.6595716529892345914, -0.7516416929448823669 ) ) ;
#6588 = ADVANCED_FACE ( 'NONE', ( #9942, #1932 ), #9695, .T. ) ;
#6589 = EDGE_LOOP ( 'NONE', ( #5486, #11021 ) ) ;
#6590 = EDGE_CURVE ( 'NONE', #15938, #24485, #23318, .T. ) ;
#6591 = CARTESIAN_POINT ( 'NONE',  ( 37.69796330110505522, -12.50384086642191228, 73.09843995877329803 ) ) ;
#6592 = LINE ( 'NONE', #10470, #3171 ) ;
#6593 = CARTESIAN_POINT ( 'NONE',  ( 37.25202387243752611, -5.213682088886100630, 70.00779233799264034 ) ) ;
#6594 = ORIENTED_EDGE ( 'NONE', *, *, #19634, .F. ) ;
#6595 = CARTESIAN_POINT ( 'NONE',  ( 39.02088643472237095, -18.91368208888609814, 69.02690120949091579 ) ) ;
#6596 = ORIENTED_EDGE ( 'NONE', *, *, #16991, .T. ) ;
#6597 = LINE ( 'NONE', #21807, #24659 ) ;
#6598 = DIRECTION ( 'NONE',  ( 2.690219486203388234E-15, -0.8967398287344627850, -0.4425581086832399147 ) ) ;
#6599 = CARTESIAN_POINT ( 'NONE',  ( 38.93987200065210175, -8.803840866421911215, 72.33091598616827866 ) ) ;
#6600 = ORIENTED_EDGE ( 'NONE', *, *, #9470, .T. ) ;
#6601 = ORIENTED_EDGE ( 'NONE', *, *, #16404, .T. ) ;
#6602 = DIRECTION ( 'NONE',  ( 0.000000000000000000, 1.000000000000000000, 0.000000000000000000 ) ) ;
#6603 = DIRECTION ( 'NONE',  ( 1.734723475976805122E-16, 3.491481338843134933E-15, 1.000000000000000000 ) ) ;
#6604 = CARTESIAN_POINT ( 'NONE',  ( 37.61123632939164452, -23.70384086642191335, 69.02690120949091579 ) ) ;
#6605 = AXIS2_PLACEMENT_3D ( 'NONE', #20985, #1266, #9147 ) ;
#6606 = DIRECTION ( 'NONE',  ( 0.000000000000000000, 0.1771812806364704007, 0.9841782327363373106 ) ) ;
#6607 = CARTESIAN_POINT ( 'NONE',  ( 38.93415946300897446, -26.11368208888610098, 73.09843995877328382 ) ) ;
#6608 = DIRECTION ( 'NONE',  ( 9.027796614315171564E-31, 1.000000000000000000, 4.694469519536151390E-16 ) ) ;
#6609 = DIRECTION ( 'NONE',  ( 2.453269466693404537E-16, -0.7071067811865489050, 0.7071067811865460184 ) ) ;
#6610 = ORIENTED_EDGE ( 'NONE', *, *, #16304, .T. ) ;
#6611 = PLANE ( 'NONE',  #5097 ) ;
#6612 = CARTESIAN_POINT ( 'NONE',  ( 44.06606138205700063, 42.82479937715250173, 82.59790614618329130 ) ) ;
#6613 = CARTESIAN_POINT ( 'NONE',  ( 37.80618814713138676, -15.70384086642190979, 69.62690120949091011 ) ) ;
#6614 = CARTESIAN_POINT ( 'NONE',  ( 0.000000000000000000, 0.000000000000000000, 0.000000000000000000 ) ) ;
#6615 = PLANE ( 'NONE',  #1770 ) ;
#6616 = AXIS2_PLACEMENT_3D ( 'NONE', #13484, #1736, #15794 ) ;
#6617 = LINE ( 'NONE', #3128, #25449 ) ;
#6618 = VECTOR ( 'NONE', #17352, 1000.000000000000000 ) ;
#6619 = CARTESIAN_POINT ( 'NONE',  ( 40.31606138205700773, -21.90577604921433874, 28.73660501626934760 ) ) ;
#6620 = CARTESIAN_POINT ( 'NONE',  ( 37.25202387243754032, -28.40384086642191619, 72.75271321436730432 ) ) ;
#6621 = CARTESIAN_POINT ( 'NONE',  ( 37.67019652925851148, -5.301844549589977973, 82.79965153790806198 ) ) ;
#6622 = VERTEX_POINT ( 'NONE', #21401 ) ;
#6623 = CARTESIAN_POINT ( 'NONE',  ( 37.33957961208646736, -27.81368208888611093, 72.81632618279320468 ) ) ;
#6624 = VERTEX_POINT ( 'NONE', #13799 ) ;
#6625 = ORIENTED_EDGE ( 'NONE', *, *, #20805, .F. ) ;
#6626 = DIRECTION ( 'NONE',  ( -1.000000000000000000, -2.999999999999999839E-15, 0.000000000000000000 ) ) ;
#6628 = EDGE_CURVE ( 'NONE', #13616, #5143, #613, .T. ) ;
#6627 = DIRECTION ( 'NONE',  ( 0.000000000000000000, -2.999999999999999839E-15, -1.000000000000000000 ) ) ;
#6629 = CARTESIAN_POINT ( 'NONE',  ( 38.63098279924288647, -4.913682088886102584, 70.22690120949091863 ) ) ;
#6630 = CARTESIAN_POINT ( 'NONE',  ( 38.26194895904383486, -7.013682088886100452, 70.24448340153877268 ) ) ;
#6631 = VERTEX_POINT ( 'NONE', #17286 ) ;
#6632 = ORIENTED_EDGE ( 'NONE', *, *, #20373, .F. ) ;
#6633 = DIRECTION ( 'NONE',  ( 0.000000000000000000, -1.000000000000000000, 3.130104260698260371E-15 ) ) ;
#6634 = DIRECTION ( 'NONE',  ( 0.000000000000000000, 2.999999999999999839E-15, 1.000000000000000000 ) ) ;
#6635 = ORIENTED_EDGE ( 'NONE', *, *, #7210, .T. ) ;
#6636 = CARTESIAN_POINT ( 'NONE',  ( 33.31606138205700773, -18.80550481115971806, 25.27912300651437150 ) ) ;
#6637 = CARTESIAN_POINT ( 'NONE',  ( 39.95015449827720744, -9.003840866421912281, 71.96809898377888715 ) ) ;
#6638 =( NAMED_UNIT ( * ) PLANE_ANGLE_UNIT ( ) SI_UNIT ( $, .RADIAN. ) );
#6639 = DIRECTION ( 'NONE',  ( 2.753529326947312927E-16, -1.000000000000000000, 3.304235192336775512E-15 ) ) ;
#6640 = ORIENTED_EDGE ( 'NONE', *, *, #8820, .T. ) ;
#6641 = ORIENTED_EDGE ( 'NONE', *, *, #23106, .F. ) ;
#6642 = AXIS2_PLACEMENT_3D ( 'NONE', #23896, #2259, #16290 ) ;
#6643 = VERTEX_POINT ( 'NONE', #15345 ) ;
#6644 = CARTESIAN_POINT ( 'NONE',  ( 45.06606138205697221, -4.349482454670840603, -5.142398479549302515 ) ) ;
#6645 = CARTESIAN_POINT ( 'NONE',  ( 36.80608444377001121, -5.313682088886100274, 70.35351908239861984 ) ) ;
#6646 =( GEOMETRIC_REPRESENTATION_CONTEXT ( 3 ) GLOBAL_UNCERTAINTY_ASSIGNED_CONTEXT ( ( #16158 ) ) GLOBAL_UNIT_ASSIGNED_CONTEXT ( ( #25249, #5687, #23585 ) ) REPRESENTATION_CONTEXT ( 'NONE', 'WORKASPACE' ) );
#6647 = LINE ( 'NONE', #14382, #6913 ) ;
#6648 = DIRECTION ( 'NONE',  ( 1.000000000000000000, 0.000000000000000000, 0.000000000000000000 ) ) ;
#6649 = CARTESIAN_POINT ( 'NONE',  ( 30.81606138205700418, -34.55876147765410167, 70.30501292737000085 ) ) ;
#6650 = DIRECTION ( 'NONE',  ( -1.000000000000000000, -1.000000000000000078E-15, 0.000000000000000000 ) ) ;
#6651 = CARTESIAN_POINT ( 'NONE',  ( 36.82041202018974957, -5.837982138606934157, 82.78530851280675051 ) ) ;
#6652 = DIRECTION ( 'NONE',  ( 1.327674326049719602E-15, -0.4425581086832399147, 0.8967398287344627850 ) ) ;
#6653 = EDGE_LOOP ( 'NONE', ( #13646, #1238, #15076, #290, #15202, #19941, #9352, #6533 ) ) ;
#6654 = ORIENTED_EDGE ( 'NONE', *, *, #245, .F. ) ;
#6655 = VECTOR ( 'NONE', #13137, 1000.000000000000000 ) ;
#6657 = ADVANCED_FACE ( 'NONE', ( #3495 ), #3743, .F. ) ;
#6656 = CARTESIAN_POINT ( 'NONE',  ( 33.31606138205700773, -22.22127907754187959, 75.30501292736998664 ) ) ;
#6658 = CARTESIAN_POINT ( 'NONE',  ( 40.55423172469004811, -28.41368208888610525, 72.05058123536539938 ) ) ;
#6659 = ADVANCED_FACE ( 'NONE', ( #4008 ), #2063, .T. ) ;
#6660 = CARTESIAN_POINT ( 'NONE',  ( 39.37952058850012804, -22.61368208888610454, 70.97781676520601479 ) ) ;
#6661 = VERTEX_POINT ( 'NONE', #5563 ) ;
#6662 = ORIENTED_EDGE ( 'NONE', *, *, #111, .T. ) ;
#6663 = AXIS2_PLACEMENT_3D ( 'NONE', #5239, #11308, #9372 ) ;
#6664 = CARTESIAN_POINT ( 'NONE',  ( 17.31606138205699708, 42.46194149498198556, 81.44836866983821722 ) ) ;
#6665 = CARTESIAN_POINT ( 'NONE',  ( 39.75915168707250302, -2.713682088886101962, 70.26145752964252722 ) ) ;
#6666 = CARTESIAN_POINT ( 'NONE',  ( 37.38336156205273397, -1.903840866421910638, 70.63227792289248441 ) ) ;
#6667 = DIRECTION ( 'NONE',  ( -0.1733269559585509378, 0.000000000000000000, -0.9848643390529188135 ) ) ;
#6668 = CARTESIAN_POINT ( 'NONE',  ( 36.36258059203031934, -7.713682088886110400, 72.86986841596736042 ) ) ;
#6669 = CYLINDRICAL_SURFACE ( 'NONE', #21371, 1.500000000000000222 ) ;
#6670 = CARTESIAN_POINT ( 'NONE',  ( 43.81606138205700063, 35.44123852234597649, 68.80501292736990138 ) ) ;
#6671 = EDGE_CURVE ( 'NONE', #11368, #22563, #11498, .T. ) ;
#6672 = DIRECTION ( 'NONE',  ( 1.000000000000000000, 3.469446951953611033E-15, 0.000000000000000000 ) ) ;
#6673 = AXIS2_PLACEMENT_3D ( 'NONE', #18288, #20079, #22264 ) ;
#6674 = CARTESIAN_POINT ( 'NONE',  ( 38.41621794735363693, -36.60729675983900222, 83.30501292737011454 ) ) ;
#6675 = PLANE ( 'NONE',  #2016 ) ;
#6676 = AXIS2_PLACEMENT_3D ( 'NONE', #23653, #17487, #15534 ) ;
#6677 = CARTESIAN_POINT ( 'NONE',  ( 38.41621794735363693, -36.60729675983900222, 83.30501292737011454 ) ) ;
#6678 = ORIENTED_EDGE ( 'NONE', *, *, #3073, .F. ) ;
#6679 = CARTESIAN_POINT ( 'NONE',  ( 40.31606138205700773, -20.56964486282017646, 75.94625445116911067 ) ) ;
#6680 = VECTOR ( 'NONE', #22768, 1000.000000000000000 ) ;
#6681 = CARTESIAN_POINT ( 'NONE',  ( 33.31606138205700773, 3.392460599465057403, 64.84545171350526971 ) ) ;
#6682 = ORIENTED_EDGE ( 'NONE', *, *, #3854, .F. ) ;
#6683 = AXIS2_PLACEMENT_3D ( 'NONE', #24808, #7054, #22889 ) ;
#6684 = EDGE_LOOP ( 'NONE', ( #19081, #14327, #8974, #18448 ) ) ;
#6685 = CARTESIAN_POINT ( 'NONE',  ( 37.50301148336529877, -14.50384086642191761, 73.69843995877327814 ) ) ;
#6686 = CARTESIAN_POINT ( 'NONE',  ( 39.38009889167650357, -24.21368208888610596, 72.75271321436730432 ) ) ;
#6687 = FACE_OUTER_BOUND ( 'NONE', #3360, .T. ) ;
#6688 = AXIS2_PLACEMENT_3D ( 'NONE', #1090, #22617, #22741 ) ;
#6689 = CARTESIAN_POINT ( 'NONE',  ( 42.81606138205700063, 22.19123852234701388, 73.80501292736992980 ) ) ;
#6690 = LINE ( 'NONE', #2437, #11062 ) ;
#6691 = ORIENTED_EDGE ( 'NONE', *, *, #8106, .F. ) ;
#6692 = DIRECTION ( 'NONE',  ( 1.000000000000000000, 0.000000000000000000, 0.000000000000000000 ) ) ;
#6693 = CYLINDRICAL_SURFACE ( 'NONE', #19908, 0.7500000000000006661 ) ;
#6694 = VECTOR ( 'NONE', #2597, 1000.000000000000000 ) ;
#6695 = CARTESIAN_POINT ( 'NONE',  ( 36.29569395875879678, -27.31368208888610027, 69.98269868914866265 ) ) ;
#6696 = ORIENTED_EDGE ( 'NONE', *, *, #3889, .F. ) ;
#6697 = CARTESIAN_POINT ( 'NONE',  ( 36.81606138205700063, 2.191238522346989903, 65.80501292737000085 ) ) ;
#6698 = DIRECTION ( 'NONE',  ( 0.000000000000000000, -2.999999999999999839E-15, -1.000000000000000000 ) ) ;
#6699 = CARTESIAN_POINT ( 'NONE',  ( 38.82593461698262871, -2.913682088886099919, 69.62690120949091011 ) ) ;
#6700 = PLANE ( 'NONE',  #642 ) ;
#6701 = CIRCLE ( 'NONE', #19462, 0.7500000000000006661 ) ;
#6702 = EDGE_CURVE ( 'NONE', #13874, #13029, #20789, .T. ) ;
#6703 = CARTESIAN_POINT ( 'NONE',  ( 36.80608444377001121, -23.31368208888610383, 70.35351908239857721 ) ) ;
#6704 = PLANE ( 'NONE',  #15985 ) ;
#6705 = AXIS2_PLACEMENT_3D ( 'NONE', #25272, #17315, #11525 ) ;
#6706 = AXIS2_PLACEMENT_3D ( 'NONE', #18065, #12022, #22044 ) ;
#6707 = DIRECTION ( 'NONE',  ( 0.000000000000000000, 1.000000000000000000, 0.000000000000000000 ) ) ;
#6708 = CARTESIAN_POINT ( 'NONE',  ( 39.31564783533279694, -25.30384086642191477, 70.72433947564850598 ) ) ;
#6709 = CARTESIAN_POINT ( 'NONE',  ( 39.75915168707250302, -8.713682088886097077, 70.26145752964252722 ) ) ;
#6710 = CARTESIAN_POINT ( 'NONE',  ( 44.81606138205700063, 41.44123852234595518, 61.30501292736988006 ) ) ;
#6711 = VECTOR ( 'NONE', #14707, 1000.000000000000000 ) ;
#6712 = ORIENTED_EDGE ( 'NONE', *, *, #16483, .T. ) ;
#6713 = CARTESIAN_POINT ( 'NONE',  ( 36.64852494920107517, -6.203840866421912459, 71.86517103874049894 ) ) ;
#6714 = EDGE_CURVE ( 'NONE', #10641, #22820, #15470, .T. ) ;
#6715 = FACE_OUTER_BOUND ( 'NONE', #9972, .T. ) ;
#6716 = ADVANCED_FACE ( 'NONE', ( #19463 ), #1803, .T. ) ;
#6717 = AXIS2_PLACEMENT_3D ( 'NONE', #3282, #15509, #11292 ) ;
#6718 = CARTESIAN_POINT ( 'NONE',  ( 37.80618814713140097, -7.913682088886107913, 73.13360434286904876 ) ) ;
#6719 = ORIENTED_EDGE ( 'NONE', *, *, #890, .F. ) ;
#6720 = CARTESIAN_POINT ( 'NONE',  ( 36.36258059203031934, -17.71368208888610596, 72.86986841596736042 ) ) ;
#6721 = EDGE_LOOP ( 'NONE', ( #11827, #21729, #21136, #13228 ) ) ;
#6722 = CYLINDRICAL_SURFACE ( 'NONE', #15647, 1.750000000000001554 ) ;
#6723 = EDGE_CURVE ( 'NONE', #2101, #21215, #12010, .T. ) ;
#6724 = CARTESIAN_POINT ( 'NONE',  ( 36.31606138205698642, -9.274586591516587930, 29.12776117315710067 ) ) ;
#6725 = CARTESIAN_POINT ( 'NONE',  ( 37.38336156205273397, -13.90384086642191264, 70.63227792289247020 ) ) ;
#6726 = EDGE_CURVE ( 'NONE', #4631, #2880, #17930, .T. ) ;
#6727 = ADVANCED_FACE ( 'NONE', ( #12521 ), #8128, .T. ) ;
#6728 =( GEOMETRIC_REPRESENTATION_CONTEXT ( 3 ) GLOBAL_UNCERTAINTY_ASSIGNED_CONTEXT ( ( #8504 ) ) GLOBAL_UNIT_ASSIGNED_CONTEXT ( ( #3333, #18933, #7076 ) ) REPRESENTATION_CONTEXT ( 'NONE', 'WORKASPACE' ) );
#6729 = CARTESIAN_POINT ( 'NONE',  ( 36.31606138205700773, -19.34822312381090370, 24.15308711316412627 ) ) ;
#6730 = ORIENTED_EDGE ( 'NONE', *, *, #18283, .F. ) ;
#6731 = CARTESIAN_POINT ( 'NONE',  ( 32.81606138205700773, 34.92314894770294131, 80.37823623207323465 ) ) ;
#6732 = DIRECTION ( 'NONE',  ( 0.000000000000000000, -2.999999999999999839E-15, -1.000000000000000000 ) ) ;
#6733 = CARTESIAN_POINT ( 'NONE',  ( 40.77203464402485622, -15.10384086642191548, 71.43714994484032843 ) ) ;
#6734 = CIRCLE ( 'NONE', #19073, 1.000000000000000888 ) ;
#6735 = CARTESIAN_POINT ( 'NONE',  ( 36.31606138205700773, -21.38339321089542722, 27.67811916372966863 ) ) ;
#6736 = CARTESIAN_POINT ( 'NONE',  ( 40.31606138205701484, -21.39087554181786643, 28.82307548518891238 ) ) ;
#6737 = CARTESIAN_POINT ( 'NONE',  ( 36.49096545463212493, -27.51368208888610312, 71.43714994484030001 ) ) ;
#6738 = DIRECTION ( 'NONE',  ( -1.156482317317870739E-16, -0.4425581086832400257, 0.8967398287344628960 ) ) ;
#6739 = VECTOR ( 'NONE', #1436, 1000.000000000000000 ) ;
#6740 = ADVANCED_FACE ( 'NONE', ( #24078 ), #10570, .F. ) ;
#6741 = LINE ( 'NONE', #9199, #25404 ) ;
#6742 = ADVANCED_FACE ( 'NONE', ( #21906 ), #6070, .F. ) ;
#6743 = ORIENTED_EDGE ( 'NONE', *, *, #13440, .F. ) ;
#6744 = CARTESIAN_POINT ( 'NONE',  ( 41.81606138205700063, -8.868983839943650693, 54.29715396818559725 ) ) ;
#6745 = LINE ( 'NONE', #22836, #6066 ) ;
#6746 = CARTESIAN_POINT ( 'NONE',  ( 36.80608444377002542, -16.30384086642191477, 72.40698646996133903 ) ) ;
#6747 = DIRECTION ( 'NONE',  ( 1.000000000000000000, 0.000000000000000000, 0.000000000000000000 ) ) ;
#6748 = CARTESIAN_POINT ( 'NONE',  ( 35.91606138205694521, 3.586515973360777654, -0.5067327973472466329 ) ) ;
#6749 = CYLINDRICAL_SURFACE ( 'NONE', #9422, 1.249999999999998668 ) ;
#6750 = VECTOR ( 'NONE', #10506, 1000.000000000000000 ) ;
#6751 = CARTESIAN_POINT ( 'NONE',  ( 33.31606138205700773, -20.93319939328399926, 43.78741072286599945 ) ) ;
#6752 = CARTESIAN_POINT ( 'NONE',  ( 39.02742774030101458, 0.5961591335780883627, 70.49320253461762320 ) ) ;
#6753 = DIRECTION ( 'NONE',  ( -0.9797958971132711969, -0.1642410374602840950, -0.1141266034453383288 ) ) ;
#6754 = ORIENTED_EDGE ( 'NONE', *, *, #16616, .F. ) ;
#6755 = VECTOR ( 'NONE', #25474, 1000.000000000000000 ) ;
#6756 = CARTESIAN_POINT ( 'NONE',  ( 39.95015449827720744, -24.61368208888610454, 70.79240656858104330 ) ) ;
#6757 = VERTEX_POINT ( 'NONE', #2689 ) ;
#6758 = ORIENTED_EDGE ( 'NONE', *, *, #16488, .T. ) ;
#6759 = CARTESIAN_POINT ( 'NONE',  ( 0.000000000000000000, 35.12314894770293705, 81.37823623207324886 ) ) ;
#6760 = CARTESIAN_POINT ( 'NONE',  ( 30.81606138205700418, -34.55876147765410167, 70.30501292737000085 ) ) ;
#6761 = CARTESIAN_POINT ( 'NONE',  ( 37.60469502381300089, -1.213682088886100630, 70.49320253461759478 ) ) ;
#6762 = EDGE_CURVE ( 'NONE', #14130, #22400, #20357, .T. ) ;
#6763 = CARTESIAN_POINT ( 'NONE',  ( 38.26194895904383486, 0.9863179111139001032, 70.24448340153880110 ) ) ;
#6764 = ORIENTED_EDGE ( 'NONE', *, *, #10589, .T. ) ;
#6765 = VERTEX_POINT ( 'NONE', #12387 ) ;
#6766 = CARTESIAN_POINT ( 'NONE',  ( 42.56606138205700063, -33.36905983554797217, 58.95447945960771818 ) ) ;
#6767 = CARTESIAN_POINT ( 'NONE',  ( 33.31606138205700773, 7.864187680719676443, 65.89022736311019912 ) ) ;
#6768 = ORIENTED_EDGE ( 'NONE', *, *, #18408, .T. ) ;
#6769 =( NAMED_UNIT ( * ) SI_UNIT ( $, .STERADIAN. ) SOLID_ANGLE_UNIT ( ) );
#6770 = CARTESIAN_POINT ( 'NONE',  ( 39.95015449827720744, -5.003840866421912281, 71.96809898377888715 ) ) ;
#6771 = ADVANCED_BREP_SHAPE_REPRESENTATION ( '', ( #17330, #2000 ), #23998 ) ;
#6772 = CARTESIAN_POINT ( 'NONE',  ( 38.41621794735363693, -38.10729675983899511, 83.30501292737011454 ) ) ;
#6773 =( GEOMETRIC_REPRESENTATION_CONTEXT ( 3 ) GLOBAL_UNCERTAINTY_ASSIGNED_CONTEXT ( ( #10308 ) ) GLOBAL_UNIT_ASSIGNED_CONTEXT ( ( #13225, #7419, #4438 ) ) REPRESENTATION_CONTEXT ( 'NONE', 'WORKASPACE' ) );
#6774 = FACE_OUTER_BOUND ( 'NONE', #9714, .T. ) ;
#6775 = VERTEX_POINT ( 'NONE', #4270 ) ;
#6776 = AXIS2_PLACEMENT_3D ( 'NONE', #20674, #1465, #22979 ) ;
#6777 = ORIENTED_EDGE ( 'NONE', *, *, #14135, .F. ) ;
#6778 = ORIENTED_EDGE ( 'NONE', *, *, #9594, .F. ) ;
#6779 = PLANE ( 'NONE',  #20708 ) ;
#6780 = CARTESIAN_POINT ( 'NONE',  ( 38.26194895904383486, -5.013682088886102228, 69.64448340153879258 ) ) ;
#6781 = DIRECTION ( 'NONE',  ( 1.000000000000000000, -1.301042606982604682E-30, -4.336808689942015271E-16 ) ) ;
#6782 = B_SPLINE_CURVE_WITH_KNOTS ( 'NONE', 3,
 ( #7036, #12721, #9247, #18508, #14884, #12602, #6788, #4730, #20698, #3034, #4848, #6651, #10910, #838, #22372, #5116, #20438, #18761 ),
 .UNSPECIFIED., .F., .F.,
 ( 4, 2, 2, 2, 2, 2, 2, 2, 4 ),
 ( 0.000000000000000000, 0.1249999999999964473, 0.2499999999999928946, 0.3749999999999893419, 0.4374999999999907851, 0.4999999999999922284, 0.6249999999999952260, 0.7499999999999982236, 1.000000000000000000 ),
 .UNSPECIFIED. ) ;
#6783 = FACE_OUTER_BOUND ( 'NONE', #6226, .T. ) ;
#6784 = ORIENTED_EDGE ( 'NONE', *, *, #3083, .F. ) ;
#6785 = DIRECTION ( 'NONE',  ( 0.000000000000000000, 1.000000000000000000, 0.000000000000000000 ) ) ;
#6786 = EDGE_CURVE ( 'NONE', #13846, #10306, #15970, .T. ) ;
#6787 = CARTESIAN_POINT ( 'NONE',  ( 44.81606138205700063, 28.12806996228107437, 66.30501292736992980 ) ) ;
#6788 = CARTESIAN_POINT ( 'NONE',  ( 37.32688434004231937, -5.448512656755814199, 82.80225578647099383 ) ) ;
#6789 = DIRECTION ( 'NONE',  ( 2.272188232479825545E-15, -0.7573960774932753104, 0.6529557272876933549 ) ) ;
#6790 = ORIENTED_EDGE ( 'NONE', *, *, #22629, .F. ) ;
#6791 = VERTEX_POINT ( 'NONE', #8512 ) ;
#6792 = CARTESIAN_POINT ( 'NONE',  ( 32.81606138205700773, 44.92314894770294131, 81.37823623207322044 ) ) ;
#6793 = CARTESIAN_POINT ( 'NONE',  ( 38.37017380507020192, -26.01368208888611022, 73.71602215082113219 ) ) ;
#6794 = CARTESIAN_POINT ( 'NONE',  ( 38.31606138205700063, -30.30876147765401285, 70.30501292737010033 ) ) ;
#6795 = CARTESIAN_POINT ( 'NONE',  ( 37.25260217561390874, -15.61368208888610276, 71.78268878715392987 ) ) ;
#6796 = VERTEX_POINT ( 'NONE', #22153 ) ;
#6797 = ORIENTED_EDGE ( 'NONE', *, *, #2623, .F. ) ;
#6798 = FACE_OUTER_BOUND ( 'NONE', #11554, .T. ) ;
#6799 = CARTESIAN_POINT ( 'NONE',  ( 36.87297107704152666, -1.713682088886108179, 72.49904802271743165 ) ) ;
#6800 = CARTESIAN_POINT ( 'NONE',  ( 37.31647492878124694, -0.3038408664219096056, 72.03616607671141026 ) ) ;
#6801 = FACE_OUTER_BOUND ( 'NONE', #5045, .T. ) ;
#6802 = CARTESIAN_POINT ( 'NONE',  ( 36.07789103942398867, -9.413682088886105248, 70.70992431699450265 ) ) ;
#6803 = DIRECTION ( 'NONE',  ( -1.000000000000000000, -1.148292460158763848E-16, -7.979170143241527150E-17 ) ) ;
#6804 = CARTESIAN_POINT ( 'NONE',  ( 32.81606138205700773, 35.12314894770294416, 81.37823623207324886 ) ) ;
#6805 = DIRECTION ( 'NONE',  ( -1.000000000000000000, 0.000000000000000000, 0.000000000000000000 ) ) ;
#6806 = AXIS2_PLACEMENT_3D ( 'NONE', #14430, #21784, #8258 ) ;
#6807 = EDGE_CURVE ( 'NONE', #7351, #18272, #20226, .T. ) ;
#6808 = LINE ( 'NONE', #3319, #9579 ) ;
#6809 = ADVANCED_FACE ( 'NONE', ( #22032, #10447 ), #13928, .T. ) ;
#6810 = CARTESIAN_POINT ( 'NONE',  ( 40.30346352106939634, -6.861678099637780193, 82.66238161308596943 ) ) ;
#6811 = CARTESIAN_POINT ( 'NONE',  ( 33.33121445922205339, -32.87633672316712108, 59.29685926994373091 ) ) ;
#6812 = EDGE_CURVE ( 'NONE', #10765, #18894, #10915, .T. ) ;
#6813 = CARTESIAN_POINT ( 'NONE',  ( 32.81606138205700773, -27.17722769842920272, 59.42551550655435477 ) ) ;
#6814 = ORIENTED_EDGE ( 'NONE', *, *, #22457, .T. ) ;
#6815 = CARTESIAN_POINT ( 'NONE',  ( 40.05426416818898616, -21.26921683217381798, 75.85227166721355729 ) ) ;
#6816 = DIRECTION ( 'NONE',  ( 1.000000000000000000, -1.717186273645140974E-30, 2.471224469859308882E-30 ) ) ;
#6817 = ORIENTED_EDGE ( 'NONE', *, *, #20893, .F. ) ;
#6818 = ORIENTED_EDGE ( 'NONE', *, *, #20976, .T. ) ;
#6819 = CARTESIAN_POINT ( 'NONE',  ( 36.36258059203030513, -17.90384086642190908, 69.89063713639259845 ) ) ;
#6820 = CARTESIAN_POINT ( 'NONE',  ( 37.69796330110504101, -21.11368208888610454, 69.66206559358661821 ) ) ;
#6821 = DIRECTION ( 'NONE',  ( 0.000000000000000000, -0.3299742535180970049, 0.9439899321577400748 ) ) ;
#6822 = DIRECTION ( 'NONE',  ( -1.000000000000000000, -1.734723475976799945E-16, 1.734723475976814737E-16 ) ) ;
#6823 = ORIENTED_EDGE ( 'NONE', *, *, #10661, .F. ) ;
#6824 = DIRECTION ( 'NONE',  ( -1.000000000000000000, 0.000000000000000000, 0.000000000000000000 ) ) ;
#6825 = DIRECTION ( 'NONE',  ( 0.1803747433772529551, 0.9835979625596985576, 0.000000000000000000 ) ) ;
#6826 = CARTESIAN_POINT ( 'NONE',  ( 36.89935272106205133, -0.4038408664219194089, 73.23812341099225875 ) ) ;
#6827 = ORIENTED_EDGE ( 'NONE', *, *, #128, .F. ) ;
#6828 = DIRECTION ( 'NONE',  ( 0.000000000000000000, -0.5706330172266952383, 0.8212051873014186709 ) ) ;
#6829 = DIRECTION ( 'NONE',  ( 0.000000000000000000, -0.7516416929448823669, -0.6595716529892345914 ) ) ;
#6830 = CARTESIAN_POINT ( 'NONE',  ( 39.38009889167650357, -0.2136820888861065693, 72.75271321436733274 ) ) ;
#6831 = DIRECTION ( 'NONE',  ( 1.000000000000000000, -5.158740922465810421E-30, -5.611568911007197376E-44 ) ) ;
#6832 = CARTESIAN_POINT ( 'NONE',  ( 37.69796330110504101, -21.11368208888610098, 69.66206559358663242 ) ) ;
#6833 = CARTESIAN_POINT ( 'NONE',  ( 32.81606138205700773, 35.92314894770293421, 79.37823623207323465 ) ) ;
#6834 = FACE_OUTER_BOUND ( 'NONE', #11735, .T. ) ;
#6835 = CARTESIAN_POINT ( 'NONE',  ( 37.25260217561390874, -16.00384086642191050, 70.97781676520601479 ) ) ;
#6836 = CARTESIAN_POINT ( 'NONE',  ( 36.49096545463212493, -3.513682088886103116, 71.43714994484035685 ) ) ;
#6837 = DIRECTION ( 'NONE',  ( 0.000000000000000000, 3.469446951953613400E-15, 1.000000000000000000 ) ) ;
#6838 = ORIENTED_EDGE ( 'NONE', *, *, #19490, .F. ) ;
#6839 = CARTESIAN_POINT ( 'NONE',  ( 38.26194895904384907, -6.603840866421916367, 73.11602215082118050 ) ) ;
#6840 = CARTESIAN_POINT ( 'NONE',  ( 38.31606138205700063, 38.69123852234598360, 71.30501292737018559 ) ) ;
#6841 = EDGE_CURVE ( 'NONE', #24067, #14769, #7372, .T. ) ;
#6842 = CARTESIAN_POINT ( 'NONE',  ( 39.95015449827720744, -4.613682088886104538, 70.79240656858107172 ) ) ;
#6843 = ORIENTED_EDGE ( 'NONE', *, *, #2982, .F. ) ;
#6844 = CARTESIAN_POINT ( 'NONE',  ( 37.50301148336529167, -11.11368208888610276, 69.06206559358666652 ) ) ;
#6845 = ORIENTED_EDGE ( 'NONE', *, *, #1540, .T. ) ;
#6846 = CARTESIAN_POINT ( 'NONE',  ( 31.81606138205700418, 28.12806996228107437, 66.30501292736992980 ) ) ;
#6847 = CARTESIAN_POINT ( 'NONE',  ( 37.12184278917507640, -12.10384086642191193, 71.32335560751961623 ) ) ;
#6848 = LINE ( 'NONE', #20774, #9788 ) ;
#6849 = ORIENTED_EDGE ( 'NONE', *, *, #21665, .F. ) ;
#6850 = CARTESIAN_POINT ( 'NONE',  ( 35.14099152588522657, -10.60718113818700026, 84.30501292737000085 ) ) ;
#6851 = LINE ( 'NONE', #22442, #2168 ) ;
#6852 = CARTESIAN_POINT ( 'NONE',  ( 40.55423172469004101, -17.20384086642191335, 70.70992431699450265 ) ) ;
#6853 = DIRECTION ( 'NONE',  ( 0.000000000000000000, 0.8191520442889929088, 0.5735764363510447161 ) ) ;
#6854 =( LENGTH_UNIT ( ) NAMED_UNIT ( * ) SI_UNIT ( .MILLI., .METRE. ) );
#6855 = CARTESIAN_POINT ( 'NONE',  ( 39.95015449827720744, -18.61368208888610454, 70.79240656858105751 ) ) ;
#6856 = CARTESIAN_POINT ( 'NONE',  ( 31.91606138205697363, -3.854803714928949798, -5.706129749257958572 ) ) ;
#6857 = CARTESIAN_POINT ( 'NONE',  ( 33.56606138205700773, 41.44123852234595518, 61.30501292736988006 ) ) ;
#6858 = EDGE_CURVE ( 'NONE', #22022, #22279, #502, .T. ) ;
#6859 = VERTEX_POINT ( 'NONE', #9288 ) ;
#6860 = DIRECTION ( 'NONE',  ( -6.056754644426120895E-31, -1.000000000000000000, -4.914813388431354887E-16 ) ) ;
#6861 = ADVANCED_FACE ( 'NONE', ( #1277 ), #11211, .T. ) ;
#6862 = CARTESIAN_POINT ( 'NONE',  ( 44.81606138205700063, 40.39281886181299797, 66.30501292737000085 ) ) ;
#6863 = CARTESIAN_POINT ( 'NONE',  ( 36.87297107704151244, -17.90384086642190553, 70.26145752964255564 ) ) ;
#6864 = AXIS2_PLACEMENT_3D ( 'NONE', #18369, #2639, #22229 ) ;
#6865 = DIRECTION ( 'NONE',  ( 0.000000000000000000, 0.000000000000000000, 1.000000000000000000 ) ) ;
#6866 = DIRECTION ( 'NONE',  ( 0.000000000000000000, 1.000000000000000000, -2.999999999999999839E-15 ) ) ;
#6867 = EDGE_CURVE ( 'NONE', #1130, #19369, #1846, .T. ) ;
#6868 = CARTESIAN_POINT ( 'NONE',  ( 36.80608444377001121, -25.31368208888610383, 70.35351908239857721 ) ) ;
#6869 = AXIS2_PLACEMENT_3D ( 'NONE', #10755, #6873, #8947 ) ;
#6870 = CARTESIAN_POINT ( 'NONE',  ( 35.52536905565747105, -37.40916500673439771, 84.30501292737011454 ) ) ;
#6871 = DIRECTION ( 'NONE',  ( -1.836970198721029688E-16, -2.999999999999999839E-15, -1.000000000000000000 ) ) ;
#6872 = CARTESIAN_POINT ( 'NONE',  ( 38.82593461698265003, -24.70384086642191690, 73.13360434286902034 ) ) ;
#6873 = DIRECTION ( 'NONE',  ( 0.000000000000000000, 0.6568589528324747517, -0.7540134720837718962 ) ) ;
#6874 = VERTEX_POINT ( 'NONE', #22411 ) ;
#6875 = EDGE_CURVE ( 'NONE', #2367, #20177, #23670, .T. ) ;
#6876 = CARTESIAN_POINT ( 'NONE',  ( 38.93415946300897446, -22.11368208888610454, 73.09843995877329803 ) ) ;
#6877 = ORIENTED_EDGE ( 'NONE', *, *, #6841, .F. ) ;
#6878 = ORIENTED_EDGE ( 'NONE', *, *, #1686, .F. ) ;
#6879 = CARTESIAN_POINT ( 'NONE',  ( 44.81606138205700063, -36.30035594811090505, 74.91924054225879104 ) ) ;
#6880 = FACE_OUTER_BOUND ( 'NONE', #21998, .T. ) ;
#6881 = CARTESIAN_POINT ( 'NONE',  ( 39.37952058850012804, -0.6136820888861006518, 70.97781676520601479 ) ) ;
#6882 = CARTESIAN_POINT ( 'NONE',  ( 39.24876120206129571, -28.90384086642191264, 72.12822762946746025 ) ) ;
#6883 = VERTEX_POINT ( 'NONE', #7078 ) ;
#6884 = ORIENTED_EDGE ( 'NONE', *, *, #11715, .F. ) ;
#6885 = DIRECTION ( 'NONE',  ( 0.000000000000000000, -0.7516416929448823669, -0.6595716529892345914 ) ) ;
#6886 = DIRECTION ( 'NONE',  ( -1.000000000000000000, 0.000000000000000000, 0.000000000000000000 ) ) ;
#6887 = ORIENTED_EDGE ( 'NONE', *, *, #11175, .T. ) ;
#6888 =( LENGTH_UNIT ( ) NAMED_UNIT ( * ) SI_UNIT ( .MILLI., .METRE. ) );
#6889 = CARTESIAN_POINT ( 'NONE',  ( 39.38009889167648936, -1.403840866421906419, 70.00779233799264034 ) ) ;
#6890 = CIRCLE ( 'NONE', #25381, 1.000000000000000888 ) ;
#6891 = AXIS2_PLACEMENT_3D ( 'NONE', #3891, #11765, #19599 ) ;
#6892 = AXIS2_PLACEMENT_3D ( 'NONE', #1115, #857, #9004 ) ;
#6893 = DIRECTION ( 'NONE',  ( 0.9063205284231096170, -0.3470338693031059241, -0.2411443412468348979 ) ) ;
#6894 = DIRECTION ( 'NONE',  ( -1.000000000000000000, -1.956963323498894821E-16, 5.870889970496684443E-31 ) ) ;
#6895 = ORIENTED_EDGE ( 'NONE', *, *, #23266, .T. ) ;
#6896 = ORIENTED_EDGE ( 'NONE', *, *, #20605, .F. ) ;
#6897 = EDGE_CURVE ( 'NONE', #9931, #2758, #1139, .T. ) ;
#6898 = EDGE_LOOP ( 'NONE', ( #19926, #4483, #19609, #20947 ) ) ;
#6899 = DIRECTION ( 'NONE',  ( 0.000000000000000000, -1.000000000000000000, 0.000000000000000000 ) ) ;
#6900 = EDGE_CURVE ( 'NONE', #22327, #3194, #17003, .T. ) ;
#6901 = CARTESIAN_POINT ( 'NONE',  ( 39.95015449827720744, -0.6136820888861040935, 70.79240656858107172 ) ) ;
#6902 = DIRECTION ( 'NONE',  ( -1.000000000000000000, 0.000000000000000000, 0.000000000000000000 ) ) ;
#6903 = EDGE_CURVE ( 'NONE', #1510, #22006, #10515, .T. ) ;
#6904 = LINE ( 'NONE', #19014, #9176 ) ;
#6905 = EDGE_CURVE ( 'NONE', #12138, #24313, #5153, .T. ) ;
#6906 = EDGE_CURVE ( 'NONE', #21318, #64, #10705, .T. ) ;
#6907 = CARTESIAN_POINT ( 'NONE',  ( 35.81606138205700063, -31.05876147765399864, 75.30501292737010033 ) ) ;
#6908 = CARTESIAN_POINT ( 'NONE',  ( 44.81606138205700063, 40.39281886181299797, 80.75501292736983316 ) ) ;
#6909 = CIRCLE ( 'NONE', #4448, 1.250000000000000888 ) ;
#6910 = DIRECTION ( 'NONE',  ( 0.000000000000000000, 1.000000000000000000, -2.999999999999999839E-15 ) ) ;
#6911 = LINE ( 'NONE', #12844, #1557 ) ;
#6912 = AXIS2_PLACEMENT_3D ( 'NONE', #21946, #4562, #9979 ) ;
#6913 = VECTOR ( 'NONE', #14508, 1000.000000000000000 ) ;
#6914 = ADVANCED_FACE ( 'NONE', ( #18551 ), #24836, .T. ) ;
#6915 = DIRECTION ( 'NONE',  ( 0.000000000000000000, -1.000000000000000000, 3.491481338843135327E-15 ) ) ;
#6916 = EDGE_LOOP ( 'NONE', ( #10467, #12054, #20297, #8717 ) ) ;
#6917 = ORIENTED_EDGE ( 'NONE', *, *, #7387, .F. ) ;
#6918 = PLANE ( 'NONE',  #17782 ) ;
#6919 = FACE_OUTER_BOUND ( 'NONE', #10445, .T. ) ;
#6920 = CARTESIAN_POINT ( 'NONE',  ( 39.24876120206128860, -18.71368208888610241, 70.63227792289245599 ) ) ;
#6921 = ORIENTED_EDGE ( 'NONE', *, *, #15258, .T. ) ;
#6922 = ORIENTED_EDGE ( 'NONE', *, *, #4697, .T. ) ;
#6923 = PLANE ( 'NONE',  #22732 ) ;
#6924 = EDGE_LOOP ( 'NONE', ( #11359, #2052 ) ) ;
#6925 = CARTESIAN_POINT ( 'NONE',  ( 36.64852494920107517, -1.413682088886102806, 70.89533451361948835 ) ) ;
#6926 = CARTESIAN_POINT ( 'NONE',  ( 36.68196826583682935, -22.00384086642191406, 70.79240656858107172 ) ) ;
#6927 = PLANE ( 'NONE',  #16957 ) ;
#6928 = EDGE_CURVE ( 'NONE', #13507, #203, #13012, .T. ) ;
#6929 = CARTESIAN_POINT ( 'NONE',  ( 36.11133435605973574, -11.61368208888610454, 72.15350918040385864 ) ) ;
#6930 = DIRECTION ( 'NONE',  ( 9.887484856639309956E-17, -0.9841782327363374216, 0.1771812806364704285 ) ) ;
#6931 = CIRCLE ( 'NONE', #13120, 4.000000000000003553 ) ;
#6932 = CARTESIAN_POINT ( 'NONE',  ( 35.81606138205700063, -31.05876147765399864, 74.30501292737010033 ) ) ;
#6933 = CARTESIAN_POINT ( 'NONE',  ( 30.81606138205700418, 40.39281886181299797, 83.30501292736984453 ) ) ;
#6934 = FACE_OUTER_BOUND ( 'NONE', #17279, .T. ) ;
#6935 = CARTESIAN_POINT ( 'NONE',  ( 38.44711690269065940, -5.204193249396280585, 82.80001292736993435 ) ) ;
#6936 = CARTESIAN_POINT ( 'NONE',  ( 33.31606138205700773, -33.36512800456291217, 60.17493404035838012 ) ) ;
#6937 =( GEOMETRIC_REPRESENTATION_CONTEXT ( 3 ) GLOBAL_UNCERTAINTY_ASSIGNED_CONTEXT ( ( #18240 ) ) GLOBAL_UNIT_ASSIGNED_CONTEXT ( ( #19502, #17076, #3404 ) ) REPRESENTATION_CONTEXT ( 'NONE', 'WORKASPACE' ) );
#6938 = CARTESIAN_POINT ( 'NONE',  ( 43.81606138205700063, 39.19123852234599070, 72.05501292736988717 ) ) ;
#6939 = ORIENTED_EDGE ( 'NONE', *, *, #18851, .F. ) ;
#6940 = DIRECTION ( 'NONE',  ( 0.000000000000000000, -2.999999999999999839E-15, -1.000000000000000000 ) ) ;
#6941 = CARTESIAN_POINT ( 'NONE',  ( 40.31606138205700773, 5.691238522346986350, 65.51211970855653988 ) ) ;
#6942 = ORIENTED_EDGE ( 'NONE', *, *, #4082, .T. ) ;
#6943 = VERTEX_POINT ( 'NONE', #22539 ) ;
#6944 = CARTESIAN_POINT ( 'NONE',  ( 35.86008812008917346, -14.10384086642191548, 71.32335560751961623 ) ) ;
#6945 = AXIS2_PLACEMENT_3D ( 'NONE', #24755, #5449, #1323 ) ;
#6946 = CARTESIAN_POINT ( 'NONE',  ( 39.95015449827720744, -22.61368208888610809, 70.79240656858105751 ) ) ;
#6947 = DIRECTION ( 'NONE',  ( -0.000000000000000000, -3.469446951953613400E-15, -1.000000000000000000 ) ) ;
#6948 = EDGE_CURVE ( 'NONE', #7542, #7272, #11080, .T. ) ;
#6949 = AXIS2_PLACEMENT_3D ( 'NONE', #9542, #17390, #23686 ) ;
#6950 = EDGE_CURVE ( 'NONE', #10501, #18087, #8770, .T. ) ;
#6951 = CARTESIAN_POINT ( 'NONE',  ( 44.31606138205700063, -20.55619265724211076, 44.11584019928223910 ) ) ;
#6952 = SHAPE_REPRESENTATION_RELATIONSHIP ( 'NONE' , 'NONE' ,  #24379, #8595 ) ;
#6953 = ORIENTED_EDGE ( 'NONE', *, *, #1500, .F. ) ;
#6954 = CARTESIAN_POINT ( 'NONE',  ( 30.81606138205705037, -30.46100403034036219, 72.05704881431053366 ) ) ;
#6955 = FACE_OUTER_BOUND ( 'NONE', #10604, .T. ) ;
#6956 = CARTESIAN_POINT ( 'NONE',  ( 38.37017380507020192, -26.01368208888611022, 73.71602215082113219 ) ) ;
#6957 = ORIENTED_EDGE ( 'NONE', *, *, #23871, .F. ) ;
#6958 = AXIS2_PLACEMENT_3D ( 'NONE', #21015, #5297, #15080 ) ;
#6959 = DIRECTION ( 'NONE',  ( -3.469446951953614978E-15, -9.938893903907229794E-15, -1.000000000000000000 ) ) ;
#6960 = DIRECTION ( 'NONE',  ( 8.758115402030106693E-47, -1.000000000000000000, 3.469446951953613400E-15 ) ) ;
#6961 = CARTESIAN_POINT ( 'NONE',  ( 37.25202387243752611, -1.213682088886100630, 70.00779233799264034 ) ) ;
#6962 = DIRECTION ( 'NONE',  ( 1.000000000000000000, -6.018531076210131309E-31, -1.734723475976804876E-16 ) ) ;
#6963 = CARTESIAN_POINT ( 'NONE',  ( 38.26194895904383486, -23.01368208888609956, 69.64448340153877837 ) ) ;
#6964 = DIRECTION ( 'NONE',  ( -1.000000000000000000, 0.000000000000000000, 0.000000000000000000 ) ) ;
#6965 = EDGE_CURVE ( 'NONE', #14256, #11106, #15056, .T. ) ;
#6966 = LINE ( 'NONE', #1150, #22366 ) ;
#6967 = VECTOR ( 'NONE', #19309, 1000.000000000000000 ) ;
#6968 = CARTESIAN_POINT ( 'NONE',  ( 38.00113996487112189, -21.70384086642190979, 70.22690120949090442 ) ) ;
#6969 = CARTESIAN_POINT ( 'NONE',  ( 37.25202387243752611, -7.213682088886102406, 70.00779233799264034 ) ) ;
#6970 = ORIENTED_EDGE ( 'NONE', *, *, #3752, .F. ) ;
#6971 = DIRECTION ( 'NONE',  ( 1.000000000000000000, 2.999999999999999839E-15, 0.000000000000000000 ) ) ;
#6972 = VERTEX_POINT ( 'NONE', #16875 ) ;
#6973 = VECTOR ( 'NONE', #464, 1000.000000000000000 ) ;
#6974 = CARTESIAN_POINT ( 'NONE',  ( 38.37017380507018771, -5.603840866421908373, 69.64448340153879258 ) ) ;
#6975 = VECTOR ( 'NONE', #16454, 1000.000000000000000 ) ;
#6976 = CARTESIAN_POINT ( 'NONE',  ( 38.37017380507020192, -4.013682088886107557, 73.11602215082118050 ) ) ;
#6977 = VERTEX_POINT ( 'NONE', #4889 ) ;
#6978 = CARTESIAN_POINT ( 'NONE',  ( 38.37017380507020192, -10.01368208888611022, 73.71602215082116061 ) ) ;
#6979 = ORIENTED_EDGE ( 'NONE', *, *, #20058, .F. ) ;
#6980 = DIRECTION ( 'NONE',  ( 1.000000000000000000, 2.751104698760144965E-15, -1.228345504986737969E-16 ) ) ;
#6981 = EDGE_CURVE ( 'NONE', #12466, #25158, #12768, .T. ) ;
#6982 = CARTESIAN_POINT ( 'NONE',  ( 39.02742774030101458, -9.403840866421907307, 70.49320253461759478 ) ) ;
#6983 = EDGE_CURVE ( 'NONE', #14092, #20720, #18935, .T. ) ;
#6984 = DIRECTION ( 'NONE',  ( -1.000000000000000000, 0.000000000000000000, 0.000000000000000000 ) ) ;
#6985 = EDGE_LOOP ( 'NONE', ( #17495, #17075, #21838, #6635 ) ) ;
#6986 = DIRECTION ( 'NONE',  ( -1.000000000000000000, -1.518641380243644581E-16, -1.055262346480601087E-16 ) ) ;
#6987 = CARTESIAN_POINT ( 'NONE',  ( 40.81606138205700773, -31.05876147765399864, 75.30501292737010033 ) ) ;
#6988 = CARTESIAN_POINT ( 'NONE',  ( 36.98690846071097127, -13.80384086642191122, 69.45876917294175712 ) ) ;
#6989 = PLANE ( 'NONE',  #7081 ) ;
#6990 = CARTESIAN_POINT ( 'NONE',  ( 39.75915168707250302, -22.71368208888610241, 70.26145752964251301 ) ) ;
#6991 = DIRECTION ( 'NONE',  ( 0.000000000000000000, 0.000000000000000000, -1.000000000000000000 ) ) ;
#6992 = PLANE ( 'NONE',  #16744 ) ;
#6993 = AXIS2_PLACEMENT_3D ( 'NONE', #13849, #9863, #3933 ) ;
#6994 = VERTEX_POINT ( 'NONE', #1013 ) ;
#6995 = DIRECTION ( 'NONE',  ( -1.327674326049721180E-15, 0.4425581086832404143, -0.8967398287344625629 ) ) ;
#6996 = CARTESIAN_POINT ( 'NONE',  ( 45.81606138205700063, -26.97987052895604876, 80.55501292737007191 ) ) ;
#6997 = ADVANCED_FACE ( 'NONE', ( #5019 ), #12890, .T. ) ;
#6998 = CARTESIAN_POINT ( 'NONE',  ( 38.93415946300897446, -7.503840866421907840, 69.66206559358664663 ) ) ;
#6999 = CARTESIAN_POINT ( 'NONE',  ( 0.000000000000000000, 0.000000000000000000, 0.000000000000000000 ) ) ;
#7000 = DIRECTION ( 'NONE',  ( -8.758115402030106693E-47, 1.000000000000000000, -3.469446951953613400E-15 ) ) ;
#7001 = CARTESIAN_POINT ( 'NONE',  ( 39.29254315202756231, -26.81368208888610027, 69.94417936956671156 ) ) ;
#7002 =( REPRESENTATION_RELATIONSHIP ('NONE','NONE', #17377, #9445 ) REPRESENTATION_RELATIONSHIP_WITH_TRANSFORMATION ( #5325 )SHAPE_REPRESENTATION_RELATIONSHIP( ) );
#7003 = DIRECTION ( 'NONE',  ( 4.584595141645219056E-18, 0.5706330172266919076, -0.8212051873014208914 ) ) ;
#7004 = CARTESIAN_POINT ( 'NONE',  ( 38.37017380507018771, -25.60384086642190837, 69.64448340153876416 ) ) ;
#7005 = PLANE ( 'NONE',  #13064 ) ;
#7006 = CARTESIAN_POINT ( 'NONE',  ( 39.82603832034400426, -22.31368208888610738, 72.40698646996133903 ) ) ;
#7007 = ORIENTED_EDGE ( 'NONE', *, *, #19396, .T. ) ;
#7008 = EDGE_LOOP ( 'NONE', ( #4799, #16892, #22140, #6198 ) ) ;
#7009 = CARTESIAN_POINT ( 'NONE',  ( 31.81606138205700418, 38.19123852234599070, 73.05501292736988717 ) ) ;
#7010 = FACE_OUTER_BOUND ( 'NONE', #24853, .T. ) ;
#7011 = VECTOR ( 'NONE', #6189, 1000.000000000000000 ) ;
#7012 = CARTESIAN_POINT ( 'NONE',  ( 38.93987200065210175, -28.80384086642191477, 72.33091598616823603 ) ) ;
#7013 = CARTESIAN_POINT ( 'NONE',  ( 39.24876120206128860, 1.286317911113898260, 70.63227792289248441 ) ) ;
#7014 = ORIENTED_EDGE ( 'NONE', *, *, #14823, .T. ) ;
#7015 = ORIENTED_EDGE ( 'NONE', *, *, #25189, .F. ) ;
#7016 = DIRECTION ( 'NONE',  ( 0.000000000000000000, 1.000000000000000000, -2.999999999999999839E-15 ) ) ;
#7017 = CARTESIAN_POINT ( 'NONE',  ( 43.82106138205700319, 3.913219763917289651, 6.295309157738977035 ) ) ;
#7018 = ORIENTED_EDGE ( 'NONE', *, *, #10135, .T. ) ;
#7019 = PRESENTATION_STYLE_ASSIGNMENT (( #14743 ) ) ;
#7020 = CARTESIAN_POINT ( 'NONE',  ( 36.80608444377001831, -6.303840866421912104, 72.40698646996136745 ) ) ;
#7021 = CYLINDRICAL_SURFACE ( 'NONE', #2225, 0.5000000000000004441 ) ;
#7022 = CARTESIAN_POINT ( 'NONE',  ( 33.40064408022072939, 41.43850569188389699, 79.37823623207322044 ) ) ;
#7023 = EDGE_LOOP ( 'NONE', ( #20987, #2869, #13300, #19655 ) ) ;
#7024 = VERTEX_POINT ( 'NONE', #18799 ) ;
#7025 = ORIENTED_EDGE ( 'NONE', *, *, #17415, .T. ) ;
#7026 = DIRECTION ( 'NONE',  ( 1.000000000000000000, 1.734723475976805122E-16, 0.000000000000000000 ) ) ;
#7027 = VECTOR ( 'NONE', #19712, 1000.000000000000000 ) ;
#7028 = CARTESIAN_POINT ( 'NONE',  ( 39.95015449827720744, -2.613682088886105870, 70.79240656858107172 ) ) ;
#7029 = EDGE_CURVE ( 'NONE', #21730, #17659, #5784, .T. ) ;
#7030 = DIRECTION ( 'NONE',  ( 0.000000000000000000, -1.000000000000000000, 3.469446951953611033E-15 ) ) ;
#7031 = FACE_OUTER_BOUND ( 'NONE', #20181, .T. ) ;
#7032 = CIRCLE ( 'NONE', #10325, 1.249999999999996891 ) ;
#7033 = LINE ( 'NONE', #836, #18864 ) ;
#7034 = DIRECTION ( 'NONE',  ( 0.000000000000000000, 2.999999999999998655E-15, 1.000000000000000000 ) ) ;
#7035 = LINE ( 'NONE', #5115, #23021 ) ;
#7036 = CARTESIAN_POINT ( 'NONE',  ( 38.31606138205700063, -5.204193249396280585, 82.80501292736992980 ) ) ;
#7037 =( NAMED_UNIT ( * ) PLANE_ANGLE_UNIT ( ) SI_UNIT ( $, .RADIAN. ) );
#7038 = CARTESIAN_POINT ( 'NONE',  ( 39.81746892067405952, 42.38065457974295924, 79.52109337493037344 ) ) ;
#7039 = VERTEX_POINT ( 'NONE', #11342 ) ;
#7040 = ORIENTED_EDGE ( 'NONE', *, *, #18094, .F. ) ;
#7041 = CARTESIAN_POINT ( 'NONE',  ( 43.81606138205700063, -33.60910547091194900, 60.61426200347987248 ) ) ;
#7042 = DIRECTION ( 'NONE',  ( 0.000000000000000000, 0.7540134720837687876, 0.6568589528324780824 ) ) ;
#7043 = EDGE_CURVE ( 'NONE', #3839, #8686, #25283, .T. ) ;
#7044 = ADVANCED_FACE ( 'NONE', ( #1773 ), #21497, .F. ) ;
#7045 = CARTESIAN_POINT ( 'NONE',  ( 39.24876120206128860, -16.71368208888610241, 70.63227792289245599 ) ) ;
#7046 = ORIENTED_EDGE ( 'NONE', *, *, #11980, .T. ) ;
#7047 = ORIENTED_EDGE ( 'NONE', *, *, #19037, .T. ) ;
#7048 = DIRECTION ( 'NONE',  ( 0.000000000000000000, -1.000000000000000000, 2.999999999999999839E-15 ) ) ;
#7049 = CARTESIAN_POINT ( 'NONE',  ( 38.26194895904383486, -3.013682088886100008, 69.64448340153879258 ) ) ;
#7050 = CARTESIAN_POINT ( 'NONE',  ( 39.75915168707251723, -26.90384086642191619, 72.49904802271737481 ) ) ;
#7051 = EDGE_CURVE ( 'NONE', #8061, #821, #13643, .T. ) ;
#7052 = EDGE_CURVE ( 'NONE', #4191, #20225, #23039, .T. ) ;
#7053 = EDGE_CURVE ( 'NONE', #21433, #21711, #22029, .T. ) ;
#7054 = DIRECTION ( 'NONE',  ( -1.000000000000000000, 0.000000000000000000, 0.000000000000000000 ) ) ;
#7055 = CARTESIAN_POINT ( 'NONE',  ( 36.98690846071097837, -7.813682088886109156, 73.30173637941818754 ) ) ;
#7056 = CARTESIAN_POINT ( 'NONE',  ( 41.06606138205698642, -9.092667827980692508, 28.75914562266559926 ) ) ;
#7057 = ORIENTED_EDGE ( 'NONE', *, *, #15856, .F. ) ;
#7058 = CARTESIAN_POINT ( 'NONE',  ( 43.81606138205700063, 36.92314894770293421, 79.37823623207323465 ) ) ;
#7059 = EDGE_CURVE ( 'NONE', #180, #19523, #5405, .T. ) ;
#7060 = LINE ( 'NONE', #14537, #1121 ) ;
#7061 = EDGE_CURVE ( 'NONE', #10887, #5392, #13775, .T. ) ;
#7062 = PLANE ( 'NONE',  #25168 ) ;
#7063 = CARTESIAN_POINT ( 'NONE',  ( 43.39709375099387501, 3.108381023609330107, 6.137326095127796144 ) ) ;
#7064 = LINE ( 'NONE', #22650, #15950 ) ;
#7065 = FACE_OUTER_BOUND ( 'NONE', #17101, .T. ) ;
#7066 = ORIENTED_EDGE ( 'NONE', *, *, #3670, .T. ) ;
#7067 = CARTESIAN_POINT ( 'NONE',  ( 33.56606138205700773, 41.44123852234599070, 73.55501292736987295 ) ) ;
#7068 = EDGE_CURVE ( 'NONE', #5343, #1156, #13267, .T. ) ;
#7069 = DIRECTION ( 'NONE',  ( 0.000000000000000000, 1.000000000000000000, 0.000000000000000000 ) ) ;
#7070 = ORIENTED_EDGE ( 'NONE', *, *, #2786, .F. ) ;
#7071 = VERTEX_POINT ( 'NONE', #15696 ) ;
#7072 = CARTESIAN_POINT ( 'NONE',  ( 35.86008812008917346, -20.10384086642191548, 71.32335560751961623 ) ) ;
#7073 = CARTESIAN_POINT ( 'NONE',  ( 38.82593461698262871, -22.91368208888609459, 69.62690120949091011 ) ) ;
#7074 = DIRECTION ( 'NONE',  ( 0.000000000000000000, 1.000000000000000000, 0.000000000000000000 ) ) ;
#7075 = EDGE_CURVE ( 'NONE', #13774, #2969, #9534, .T. ) ;
#7076 =( NAMED_UNIT ( * ) SI_UNIT ( $, .STERADIAN. ) SOLID_ANGLE_UNIT ( ) );
#7077 = EDGE_LOOP ( 'NONE', ( #4422, #23654, #11079, #12328 ) ) ;
#7078 = CARTESIAN_POINT ( 'NONE',  ( 45.81606138205698642, -5.575886420685123745, -6.837621553846354949 ) ) ;
#7079 = CARTESIAN_POINT ( 'NONE',  ( 38.48938833801555148, 37.69123852234600491, 72.28987726642293410 ) ) ;
#7080 = CARTESIAN_POINT ( 'NONE',  ( 36.11133435605973574, -25.61368208888610454, 72.15350918040381600 ) ) ;
#7081 = AXIS2_PLACEMENT_3D ( 'NONE', #12926, #17805, #1809 ) ;
#7082 = ORIENTED_EDGE ( 'NONE', *, *, #13045, .F. ) ;
#7083 = VECTOR ( 'NONE', #6598, 1000.000000000000000 ) ;
#7084 = CARTESIAN_POINT ( 'NONE',  ( 38.31606138205693668, 6.548188142891439689, 4.975198841308384523 ) ) ;
#7085 = CARTESIAN_POINT ( 'NONE',  ( 40.31606138205700773, -4.357181138186123626, 83.30501292736992980 ) ) ;
#7086 = CARTESIAN_POINT ( 'NONE',  ( 39.95015449827720744, -0.6136820888861040935, 70.79240656858107172 ) ) ;
#7087 = CARTESIAN_POINT ( 'NONE',  ( 44.71606138205692105, 12.25039015348823490, 8.426307875224583910 ) ) ;
#7088 = VECTOR ( 'NONE', #12482, 1000.000000000000227 ) ;
#7089 = VERTEX_POINT ( 'NONE', #1517 ) ;
#7090 = CARTESIAN_POINT ( 'NONE',  ( 36.80608444377001121, -19.31368208888610027, 70.35351908239860563 ) ) ;
#7091 = CARTESIAN_POINT ( 'NONE',  ( 38.31606138205700063, 38.69123852234599781, 71.30501292737000085 ) ) ;
#7092 = CARTESIAN_POINT ( 'NONE',  ( 42.96606138205697789, -5.898435835062210586, -2.003809078978638247 ) ) ;
#7093 = CARTESIAN_POINT ( 'NONE',  ( 38.63098279924290068, -16.70384086642190624, 72.53360434286904024 ) ) ;
#7094 = CARTESIAN_POINT ( 'NONE',  ( 39.29254315202756231, -6.813682088886101162, 69.94417936956673998 ) ) ;
#7095 = ORIENTED_EDGE ( 'NONE', *, *, #20949, .T. ) ;
#7096 = CARTESIAN_POINT ( 'NONE',  ( 34.06606138205700773, -33.36905983554797217, 58.95447945960771818 ) ) ;
#7097 = EDGE_CURVE ( 'NONE', #9294, #19809, #23161, .T. ) ;
#7098 = EDGE_LOOP ( 'NONE', ( #1987, #14459, #22120, #716 ) ) ;
#7099 = ADVANCED_FACE ( 'NONE', ( #5535 ), #13517, .T. ) ;
#7100 = VECTOR ( 'NONE', #24551, 1000.000000000000000 ) ;
#7101 = CARTESIAN_POINT ( 'NONE',  ( 38.93415946300896024, -7.503840866421907840, 69.66206559358663242 ) ) ;
#7102 = DIRECTION ( 'NONE',  ( 0.000000000000000000, 0.8191520442889929088, 0.5735764363510447161 ) ) ;
#7103 = AXIS2_PLACEMENT_3D ( 'NONE', #20965, #14776, #13114 ) ;
#7104 = CARTESIAN_POINT ( 'NONE',  ( 38.37017380507020192, -0.01368208888610777940, 73.11602215082118050 ) ) ;
#7105 = ORIENTED_EDGE ( 'NONE', *, *, #23720, .T. ) ;
#7106 = CARTESIAN_POINT ( 'NONE',  ( 36.36258059203031934, -9.713682088886105959, 72.86986841596736042 ) ) ;
#7107 = ORIENTED_EDGE ( 'NONE', *, *, #21240, .T. ) ;
#7108 = CARTESIAN_POINT ( 'NONE',  ( 30.81606138205696155, 1.773964314019528477, -3.427682652428150067 ) ) ;
#7109 = CARTESIAN_POINT ( 'NONE',  ( 39.02742774030101458, -13.40384086642191619, 70.49320253461759478 ) ) ;
#7110 = CYLINDRICAL_SURFACE ( 'NONE', #16342, 0.4999999999999995559 ) ;
#7111 = ORIENTED_EDGE ( 'NONE', *, *, #16308, .T. ) ;
#7112 = CIRCLE ( 'NONE', #9169, 1.249999999999998668 ) ;
#7113 = CARTESIAN_POINT ( 'NONE',  ( 47.81606138205695800, 0.4548210080410876599, -1.924399266538374009 ) ) ;
#7114 = CARTESIAN_POINT ( 'NONE',  ( 38.53272007700518742, 37.69123852234600491, 72.53609335118615320 ) ) ;
#7115 = CARTESIAN_POINT ( 'NONE',  ( 36.11133435605973574, -16.00384086642191406, 70.60699637195608602 ) ) ;
#7116 = VECTOR ( 'NONE', #6168, 1000.000000000000000 ) ;
#7117 = CARTESIAN_POINT ( 'NONE',  ( 36.80559154321147020, -21.53836365414604614, 75.32286344890304974 ) ) ;
#7118 = FACE_OUTER_BOUND ( 'NONE', #23252, .T. ) ;
#7119 = CARTESIAN_POINT ( 'NONE',  ( 36.80608444377001121, -23.31368208888610383, 70.35351908239857721 ) ) ;
#7120 = CARTESIAN_POINT ( 'NONE',  ( 45.81606138205697931, -6.548589660139387369, -8.069948661059591188 ) ) ;
#7121 = CIRCLE ( 'NONE', #7550, 1.750000000000001554 ) ;
#7122 = CARTESIAN_POINT ( 'NONE',  ( 30.81606138205700418, 36.92314894770294131, 81.17823623207323180 ) ) ;
#7123 = AXIS2_PLACEMENT_3D ( 'NONE', #12182, #6240, #13972 ) ;
#7124 = ORIENTED_EDGE ( 'NONE', *, *, #7926, .F. ) ;
#7125 = CARTESIAN_POINT ( 'NONE',  ( 32.81606138205700773, 41.44123852234597649, 68.80501292736988717 ) ) ;
#7126 = CARTESIAN_POINT ( 'NONE',  ( 31.81606138205700418, 35.38401127291550097, 61.48364296169660292 ) ) ;
#7127 = AXIS2_PLACEMENT_3D ( 'NONE', #916, #13174, #20639 ) ;
#7128 = CARTESIAN_POINT ( 'NONE',  ( 39.75915168707251723, -10.90384086642191441, 72.49904802271740323 ) ) ;
#7129 = EDGE_CURVE ( 'NONE', #9062, #18567, #3975, .T. ) ;
#7130 = DIRECTION ( 'NONE',  ( 1.734723475976804876E-16, 3.491481338843135327E-15, 1.000000000000000000 ) ) ;
#7131 = CARTESIAN_POINT ( 'NONE',  ( 38.37017380507020192, -22.01368208888611022, 73.11602215082116629 ) ) ;
#7132 = ADVANCED_FACE ( 'NONE', ( #25339 ), #11849, .T. ) ;
#7133 = CARTESIAN_POINT ( 'NONE',  ( 43.31606138205700063, 4.103895195095678794, 6.341006091748962348 ) ) ;
#7134 = VECTOR ( 'NONE', #20429, 1000.000000000000114 ) ;
#7135 = EDGE_CURVE ( 'NONE', #5555, #20798, #11592, .T. ) ;
#7136 = CARTESIAN_POINT ( 'NONE',  ( 36.49096545463212493, -22.10384086642191548, 71.32335560751961623 ) ) ;
#7137 = CARTESIAN_POINT ( 'NONE',  ( 33.31606138205700773, -16.48551471403133206, 77.11349248448009064 ) ) ;
#7138 = CARTESIAN_POINT ( 'NONE',  ( 39.38009889167650357, -22.21368208888610951, 72.75271321436731853 ) ) ;
#7139 = EDGE_LOOP ( 'NONE', ( #13609, #9932, #8187, #18299 ) ) ;
#7140 = VERTEX_POINT ( 'NONE', #21122 ) ;
#7141 = CARTESIAN_POINT ( 'NONE',  ( 33.56861364504067069, 3.414468223740623642, 6.349533009087196866 ) ) ;
#7142 = AXIS2_PLACEMENT_3D ( 'NONE', #21664, #15983, #4283 ) ;
#7143 = FACE_OUTER_BOUND ( 'NONE', #23302, .T. ) ;
#7144 = CARTESIAN_POINT ( 'NONE',  ( 37.89291511884476904, -1.113682088886101207, 70.26206559358664094 ) ) ;
#7145 = ORIENTED_EDGE ( 'NONE', *, *, #17263, .F. ) ;
#7146 = EDGE_LOOP ( 'NONE', ( #10475, #6596, #4580, #12511 ) ) ;
#7147 = DIRECTION ( 'NONE',  ( -1.000000000000000000, -1.734723475976804876E-16, 1.734723475976814737E-16 ) ) ;
#7148 = EDGE_CURVE ( 'NONE', #18371, #7627, #861, .T. ) ;
#7149 = AXIS2_PLACEMENT_3D ( 'NONE', #18180, #8513, #134 ) ;
#7150 = CARTESIAN_POINT ( 'NONE',  ( 31.91606138205695942, -0.07962245140798011878, -2.393377716359348817 ) ) ;
#7151 = VERTEX_POINT ( 'NONE', #7598 ) ;
#7152 = LINE ( 'NONE', #9474, #25441 ) ;
#7153 = CARTESIAN_POINT ( 'NONE',  ( 39.95015449827720744, -3.003840866421910505, 71.96809898377888715 ) ) ;
#7154 = DIRECTION ( 'NONE',  ( 0.000000000000000000, -0.8212051873014203363, -0.5706330172266926848 ) ) ;
#7155 = VECTOR ( 'NONE', #1590, 1000.000000000000000 ) ;
#7156 = LINE ( 'NONE', #24645, #10615 ) ;
#7157 = EDGE_LOOP ( 'NONE', ( #773, #23363, #4834, #11420 ) ) ;
#7158 = ORIENTED_EDGE ( 'NONE', *, *, #15707, .F. ) ;
#7159 = ORIENTED_EDGE ( 'NONE', *, *, #7292, .T. ) ;
#7160 = CYLINDRICAL_SURFACE ( 'NONE', #9614, 1.000000000000000000 ) ;
#7161 = CARTESIAN_POINT ( 'NONE',  ( 39.38009889167650357, -0.2136820888861065693, 72.75271321436733274 ) ) ;
#7162 = ORIENTED_EDGE ( 'NONE', *, *, #1040, .T. ) ;
#7163 = DIRECTION ( 'NONE',  ( 1.156482317317870492E-16, 0.4425581086832399702, -0.8967398287344626739 ) ) ;
#7164 = CIRCLE ( 'NONE', #21132, 0.7500000000000006661 ) ;
#7165 = SHAPE_REPRESENTATION_RELATIONSHIP ( 'NONE' , 'NONE' ,  #14735, #11987 ) ;
#7166 = FACE_OUTER_BOUND ( 'NONE', #1633, .T. ) ;
#7167 = VECTOR ( 'NONE', #10831, 1000.000000000000114 ) ;
#7168 = VERTEX_POINT ( 'NONE', #15313 ) ;
#7169 = DIRECTION ( 'NONE',  ( 1.000000000000000000, 3.469446951953611033E-15, 0.000000000000000000 ) ) ;
#7170 = AXIS2_PLACEMENT_3D ( 'NONE', #12639, #22541, #6825 ) ;
#7171 = CARTESIAN_POINT ( 'NONE',  ( 32.81606138205700773, 22.19123852234699967, 69.30501292736994401 ) ) ;
#7172 = CARTESIAN_POINT ( 'NONE',  ( 31.81606138205700418, -11.72563467517899838, 72.98595903681224684 ) ) ;
#7173 = DIRECTION ( 'NONE',  ( 1.000000000000000000, 1.000000000000000078E-15, 0.000000000000000000 ) ) ;
#7174 = FACE_OUTER_BOUND ( 'NONE', #15055, .T. ) ;
#7175 = ORIENTED_EDGE ( 'NONE', *, *, #699, .T. ) ;
#7176 = VERTEX_POINT ( 'NONE', #15564 ) ;
#7177 = CARTESIAN_POINT ( 'NONE',  ( 32.81606138205700773, 6.294683054830111146, 7.131205101789720224 ) ) ;
#7178 = CARTESIAN_POINT ( 'NONE',  ( 43.38751061443460344, 3.099069811988895751, 6.135932541694130826 ) ) ;
#7179 = CARTESIAN_POINT ( 'NONE',  ( 36.64852494920107517, -0.2038408664219101829, 71.86517103874049894 ) ) ;
#7180 = CARTESIAN_POINT ( 'NONE',  ( 39.02742774030102879, -18.21368208888610241, 72.26730301774234988 ) ) ;
#7181 = ORIENTED_EDGE ( 'NONE', *, *, #19631, .T. ) ;
#7182 = ORIENTED_EDGE ( 'NONE', *, *, #17103, .T. ) ;
#7183 = EDGE_CURVE ( 'NONE', #22425, #20770, #23418, .T. ) ;
#7184 = CYLINDRICAL_SURFACE ( 'NONE', #1344, 4.000000000000000000 ) ;
#7185 = CARTESIAN_POINT ( 'NONE',  ( 37.33957961208646736, -1.813682088886107380, 72.81632618279323310 ) ) ;
#7186 = CARTESIAN_POINT ( 'NONE',  ( 38.26194895904384907, -24.60384086642191548, 73.11602215082115208 ) ) ;
#7187 = AXIS2_PLACEMENT_3D ( 'NONE', #17072, #5464, #3523 ) ;
#7188 = DIRECTION ( 'NONE',  ( 0.000000000000000000, 0.7540134720837717852, 0.6568589528324747517 ) ) ;
#7189 = VECTOR ( 'NONE', #20009, 1000.000000000000000 ) ;
#7190 = CARTESIAN_POINT ( 'NONE',  ( 40.55423172469004811, -2.413682088886103472, 72.05058123536544201 ) ) ;
#7191 = CARTESIAN_POINT ( 'NONE',  ( 44.06606138205700063, 43.35512946304240245, 81.37823623207320622 ) ) ;
#7192 = ORIENTED_EDGE ( 'NONE', *, *, #1040, .F. ) ;
#7193 = DIRECTION ( 'NONE',  ( 1.000000000000000000, 0.000000000000000000, 0.000000000000000000 ) ) ;
#7194 = PLANE ( 'NONE',  #6489 ) ;
#7195 = FACE_OUTER_BOUND ( 'NONE', #8160, .T. ) ;
#7196 = EDGE_CURVE ( 'NONE', #10628, #4783, #15825, .T. ) ;
#7197 = EDGE_CURVE ( 'NONE', #15804, #18901, #20281, .T. ) ;
#7198 = DIRECTION ( 'NONE',  ( -1.292986538149619279E-16, 0.9897030922575080769, 0.1431355622335914179 ) ) ;
#7199 = PLANE ( 'NONE',  #12680 ) ;
#7200 = EDGE_CURVE ( 'NONE', #10392, #154, #8230, .T. ) ;
#7201 = CARTESIAN_POINT ( 'NONE',  ( 33.31606138205700773, 7.864187680719676443, 65.89022736311019912 ) ) ;
#7202 = EDGE_CURVE ( 'NONE', #5640, #22871, #15324, .T. ) ;
#7203 = ORIENTED_EDGE ( 'NONE', *, *, #12874, .T. ) ;
#7204 = FACE_OUTER_BOUND ( 'NONE', #16439, .T. ) ;
#7205 = DIRECTION ( 'NONE',  ( 0.000000000000000000, 0.000000000000000000, -1.000000000000000000 ) ) ;
#7206 = ORIENTED_EDGE ( 'NONE', *, *, #20424, .T. ) ;
#7207 = EDGE_LOOP ( 'NONE', ( #6567, #15730, #8194, #15875, #23003 ) ) ;
#7208 = UNCERTAINTY_MEASURE_WITH_UNIT (LENGTH_MEASURE( 1.000000000000000082E-05 ), #12435, 'distance_accuracy_value', 'NONE');
#7209 = CARTESIAN_POINT ( 'NONE',  ( 36.98690846071097127, -17.80384086642191122, 69.45876917294175712 ) ) ;
#7210 = EDGE_CURVE ( 'NONE', #17867, #18276, #10290, .T. ) ;
#7211 = DIRECTION ( 'NONE',  ( -1.000000000000000000, -7.319250130266555251E-16, -4.595720054541213141E-15 ) ) ;
#7212 = CARTESIAN_POINT ( 'NONE',  ( 39.38009889167650357, -18.21368208888610951, 72.75271321436731853 ) ) ;
#7213 = ORIENTED_EDGE ( 'NONE', *, *, #17127, .F. ) ;
#7214 = DIRECTION ( 'NONE',  ( 0.000000000000000000, 0.7540134720837716742, 0.6568589528324746407 ) ) ;
#7215 = CARTESIAN_POINT ( 'NONE',  ( 46.91606138205695231, -23.19619402982945644, 47.16846523730003327 ) ) ;
#7216 = CARTESIAN_POINT ( 'NONE',  ( 37.61123632939165873, -21.91368208888611235, 73.73360434286898624 ) ) ;
#7217 = VECTOR ( 'NONE', #10948, 1000.000000000000114 ) ;
#7218 = ORIENTED_EDGE ( 'NONE', *, *, #24491, .T. ) ;
#7219 = FACE_OUTER_BOUND ( 'NONE', #24893, .T. ) ;
#7220 = CARTESIAN_POINT ( 'NONE',  ( 36.80608444377001121, 0.6863179111138983934, 70.35351908239860563 ) ) ;
#7221 = CARTESIAN_POINT ( 'NONE',  ( 36.31606138205700063, 37.44123852234599781, 74.30501292736988717 ) ) ;
#7222 = CARTESIAN_POINT ( 'NONE',  ( 36.68196826583682935, -13.61368208888610454, 71.96809898377888715 ) ) ;
#7223 = CARTESIAN_POINT ( 'NONE',  ( 38.31606138205700063, 39.69123852234598360, 70.30501292737018559 ) ) ;
#7224 = CARTESIAN_POINT ( 'NONE',  ( 43.31606138205700773, -21.83924545618510393, 28.60179643084731893 ) ) ;
#7225 = ADVANCED_FACE ( 'NONE', ( #16201, #6041 ), #4617, .T. ) ;
#7226 = CARTESIAN_POINT ( 'NONE',  ( 37.21915885897815457, -20.20384086642191335, 71.67976084211552745 ) ) ;
#7227 = CARTESIAN_POINT ( 'NONE',  ( 39.75915168707250302, -2.713682088886101962, 70.26145752964252722 ) ) ;
#7228 = EDGE_CURVE ( 'NONE', #15157, #4595, #2285, .T. ) ;
#7229 = EDGE_LOOP ( 'NONE', ( #23479, #22342, #6662, #4170 ) ) ;
#7230 = DIRECTION ( 'NONE',  ( -1.000000000000000078E-15, 0.9439899321577417401, 0.3299742535180921199 ) ) ;
#7231 = VERTEX_POINT ( 'NONE', #11985 ) ;
#7232 = CARTESIAN_POINT ( 'NONE',  ( 36.64852494920107517, -4.203840866421910683, 71.86517103874049894 ) ) ;
#7233 = DIRECTION ( 'NONE',  ( 0.000000000000000000, 1.000000000000000000, -2.999999999999999839E-15 ) ) ;
#7234 = EDGE_CURVE ( 'NONE', #7231, #2274, #24055, .T. ) ;
#7235 = CARTESIAN_POINT ( 'NONE',  ( 39.95015449827720744, -0.6136820888861040935, 70.79240656858107172 ) ) ;
#7236 = ORIENTED_EDGE ( 'NONE', *, *, #7644, .T. ) ;
#7237 = CARTESIAN_POINT ( 'NONE',  ( 35.86008812008917346, -11.51368208888610134, 71.43714994484034264 ) ) ;
#7238 = ORIENTED_EDGE ( 'NONE', *, *, #23339, .F. ) ;
#7239 = LINE ( 'NONE', #5183, #24679 ) ;
#7240 = CARTESIAN_POINT ( 'NONE',  ( 38.26194895904384197, -4.603840866421910150, 72.51602215082118619 ) ) ;
#7241 = DIRECTION ( 'NONE',  ( 0.000000000000000000, 0.6568589528324747517, -0.7540134720837718962 ) ) ;
#7242 = VERTEX_POINT ( 'NONE', #12491 ) ;
#7243 = DIRECTION ( 'NONE',  ( -1.000000000000000000, 0.000000000000000000, 0.000000000000000000 ) ) ;
#7244 = CARTESIAN_POINT ( 'NONE',  ( 40.81606138205700063, 8.691238522346999673, 69.30501292736998664 ) ) ;
#7245 = CARTESIAN_POINT ( 'NONE',  ( 40.26954217208372455, -18.90384086642191619, 72.86986841596734621 ) ) ;
#7246 = CARTESIAN_POINT ( 'NONE',  ( 36.31606138205700063, -20.22026907754187164, 75.50210598695683473 ) ) ;
#7247 = CARTESIAN_POINT ( 'NONE',  ( 39.95015449827720744, -22.61368208888610809, 70.79240656858105751 ) ) ;
#7248 = CARTESIAN_POINT ( 'NONE',  ( 31.91606138205695942, 0.5799492015812461876, -3.145019409304214530 ) ) ;
#7249 = ADVANCED_FACE ( 'NONE', ( #20335 ), #20203, .T. ) ;
#7250 = DIRECTION ( 'NONE',  ( 1.327674326049719602E-15, -0.4425581086832399147, 0.8967398287344627850 ) ) ;
#7251 = EDGE_LOOP ( 'NONE', ( #7681, #7442, #18934, #20003 ) ) ;
#7252 = VECTOR ( 'NONE', #24084, 1000.000000000000000 ) ;
#7253 = DIRECTION ( 'NONE',  ( 0.000000000000000000, -1.000000000000000000, 3.325260651745651169E-15 ) ) ;
#7254 = CYLINDRICAL_SURFACE ( 'NONE', #17601, 1.750000000000001554 ) ;
#7255 = CARTESIAN_POINT ( 'NONE',  ( 36.68196826583682935, -10.00384086642191406, 70.79240656858108593 ) ) ;
#7256 = DIRECTION ( 'NONE',  ( 0.000000000000000000, -1.000000000000000000, 2.999999999999999839E-15 ) ) ;
#7257 = CARTESIAN_POINT ( 'NONE',  ( 37.80618814713140097, -27.91368208888610880, 73.13360434286902034 ) ) ;
#7258 = LINE ( 'NONE', #7133, #18478 ) ;
#7259 = CARTESIAN_POINT ( 'NONE',  ( 39.75915168707251723, -24.90384086642191619, 72.49904802271737481 ) ) ;
#7260 = CARTESIAN_POINT ( 'NONE',  ( 38.05217264712879199, -5.217354499694973669, 83.30503613834979149 ) ) ;
#7261 = CARTESIAN_POINT ( 'NONE',  ( 39.75915168707250302, -20.71368208888610596, 70.26145752964251301 ) ) ;
#7262 = EDGE_LOOP ( 'NONE', ( #6719, #4720, #7587, #11279 ) ) ;
#7263 = CARTESIAN_POINT ( 'NONE',  ( 36.11133435605973574, -25.61368208888610454, 72.15350918040381600 ) ) ;
#7264 = ORIENTED_EDGE ( 'NONE', *, *, #4282, .T. ) ;
#7265 = LINE ( 'NONE', #24505, #2032 ) ;
#7266 = LINE ( 'NONE', #22974, #16580 ) ;
#7267 = CARTESIAN_POINT ( 'NONE',  ( 39.31564783533280405, -0.3136820888861025503, 72.03616607671141026 ) ) ;
#7268 = ORIENTED_EDGE ( 'NONE', *, *, #2054, .T. ) ;
#7269 = ORIENTED_EDGE ( 'NONE', *, *, #14948, .T. ) ;
#7270 = DIRECTION ( 'NONE',  ( -2.048868001712896742E-15, 0.6595716529892345914, -0.7516416929448823669 ) ) ;
#7271 = CYLINDRICAL_SURFACE ( 'NONE', #19453, 3.000000000000000888 ) ;
#7272 = VERTEX_POINT ( 'NONE', #22126 ) ;
#7273 = DIRECTION ( 'NONE',  ( 1.000000000000000000, 0.000000000000000000, 0.000000000000000000 ) ) ;
#7274 = CARTESIAN_POINT ( 'NONE',  ( 36.80608444377001831, -4.303840866421916544, 72.40698646996136745 ) ) ;
#7275 = EDGE_CURVE ( 'NONE', #19784, #18363, #10161, .T. ) ;
#7276 = ADVANCED_FACE ( 'NONE', ( #12362 ), #2536, .F. ) ;
#7277 = PLANE ( 'NONE',  #11302 ) ;
#7278 = ADVANCED_FACE ( 'NONE', ( #609 ), #21883, .T. ) ;
#7279 = DIRECTION ( 'NONE',  ( -1.734723475976804876E-16, -3.491481338843135327E-15, -1.000000000000000000 ) ) ;
#7280 = VECTOR ( 'NONE', #4342, 1000.000000000000000 ) ;
#7281 = ORIENTED_EDGE ( 'NONE', *, *, #22511, .T. ) ;
#7282 = ORIENTED_EDGE ( 'NONE', *, *, #4714, .F. ) ;
#7283 = CIRCLE ( 'NONE', #13063, 4.000000000000000000 ) ;
#7284 = AXIS2_PLACEMENT_3D ( 'NONE', #17821, #23468, #4024 ) ;
#7285 = DIRECTION ( 'NONE',  ( 3.491481338843135327E-15, -1.000000000000000000, 2.999999999999999050E-15 ) ) ;
#7286 = CARTESIAN_POINT ( 'NONE',  ( 36.80608444377001121, 0.6863179111138983934, 70.35351908239861984 ) ) ;
#7287 = ORIENTED_EDGE ( 'NONE', *, *, #8946, .F. ) ;
#7288 = CARTESIAN_POINT ( 'NONE',  ( 38.26194895904384907, -26.60384086642191548, 73.11602215082115208 ) ) ;
#7289 = CARTESIAN_POINT ( 'NONE',  ( 43.31097620093147071, -33.12114940777929917, 59.73560686274496589 ) ) ;
#7290 = ORIENTED_EDGE ( 'NONE', *, *, #21527, .T. ) ;
#7291 = PLANE ( 'NONE',  #19265 ) ;
#7292 = EDGE_CURVE ( 'NONE', #13994, #1644, #15945, .T. ) ;
#7293 = CARTESIAN_POINT ( 'NONE',  ( 43.30090830489194786, -32.87633672316712108, 59.29685926994373091 ) ) ;
#7294 = FACE_OUTER_BOUND ( 'NONE', #2086, .T. ) ;
#7295 = ORIENTED_EDGE ( 'NONE', *, *, #11580, .T. ) ;
#7296 = CARTESIAN_POINT ( 'NONE',  ( 33.31606138205700773, -12.87480755223283424, 20.78922580900563588 ) ) ;
#7297 = ORIENTED_EDGE ( 'NONE', *, *, #10977, .T. ) ;
#7298 = AXIS2_PLACEMENT_3D ( 'NONE', #23201, #15602, #3750 ) ;
#7299 = ORIENTED_EDGE ( 'NONE', *, *, #9417, .F. ) ;
#7300 = DIRECTION ( 'NONE',  ( 1.000000000000000000, 0.000000000000000000, -0.000000000000000000 ) ) ;
#7301 = DIRECTION ( 'NONE',  ( -1.000000000000000000, 0.000000000000000000, 0.000000000000000000 ) ) ;
#7302 = AXIS2_PLACEMENT_3D ( 'NONE', #8431, #24113, #16783 ) ;
#7303 = VECTOR ( 'NONE', #1882, 1000.000000000000114 ) ;
#7304 = CARTESIAN_POINT ( 'NONE',  ( 37.21915885897815457, -17.41368208888610170, 71.08074471024443142 ) ) ;
#7305 = VERTEX_POINT ( 'NONE', #10039 ) ;
#7306 = ORIENTED_EDGE ( 'NONE', *, *, #1513, .T. ) ;
#7307 = CARTESIAN_POINT ( 'NONE',  ( 40.31606138205701484, -21.38339321089542011, 27.67811916372966863 ) ) ;
#7308 = CARTESIAN_POINT ( 'NONE',  ( 30.81606138205705037, -30.65246816789535345, 72.44500581826353880 ) ) ;
#7309 = CARTESIAN_POINT ( 'NONE',  ( 39.98359781491296161, -25.20384086642191335, 70.89533451361944572 ) ) ;
#7310 = CARTESIAN_POINT ( 'NONE',  ( 42.56606138205700063, 2.740850673309605412, 6.112030963703427133 ) ) ;
#7311 = CARTESIAN_POINT ( 'NONE',  ( 39.02088643472237095, -0.9136820888861024725, 69.02690120949094421 ) ) ;
#7312 = ORIENTED_EDGE ( 'NONE', *, *, #18005, .F. ) ;
#7313 = ORIENTED_EDGE ( 'NONE', *, *, #21868, .F. ) ;
#7314 = CARTESIAN_POINT ( 'NONE',  ( 43.39709375099424449, 3.108381023609659621, 6.137326095127897396 ) ) ;
#7315 = CARTESIAN_POINT ( 'NONE',  ( 42.96606138205698500, -6.570990706613058840, -2.335727660491067503 ) ) ;
#7316 = CLOSED_SHELL ( 'NONE', ( #21757, #912, #6188, #1275, #3409, #12132, #123, #21257, #11449, #9745, #1184, #13040, #8158, #5166, #24270, #17690, #19312, #24499, #19394, #14924, #1805, #12499, #9959, #577, #12730, #8926, #13194, #13060, #17434 ) ) ;
#7317 = FACE_OUTER_BOUND ( 'NONE', #20049, .T. ) ;
#7318 = VECTOR ( 'NONE', #14090, 1000.000000000000000 ) ;
#7319 = AXIS2_PLACEMENT_3D ( 'NONE', #12752, #18919, #12270 ) ;
#7320 = CARTESIAN_POINT ( 'NONE',  ( 38.57734783014581836, -5.216950748870224253, 83.30503679799366523 ) ) ;
#7321 = CARTESIAN_POINT ( 'NONE',  ( 36.31606138205701484, -18.91453975041206093, 24.37026150481227305 ) ) ;
#7322 = ADVANCED_FACE ( 'NONE', ( #16320 ), #7984, .F. ) ;
#7323 = LINE ( 'NONE', #11712, #18495 ) ;
#7324 = VERTEX_POINT ( 'NONE', #225 ) ;
#7325 = LINE ( 'NONE', #8887, #13170 ) ;
#7326 = LINE ( 'NONE', #18924, #10 ) ;
#7327 = VERTEX_POINT ( 'NONE', #4241 ) ;
#7328 = VERTEX_POINT ( 'NONE', #6298 ) ;
#7329 = CARTESIAN_POINT ( 'NONE',  ( 36.98690846071097127, -9.803840866421911215, 69.45876917294177133 ) ) ;
#7330 = DIRECTION ( 'NONE',  ( 1.000000000000000000, 1.734723475976804876E-16, -1.734723475976814737E-16 ) ) ;
#7331 = CARTESIAN_POINT ( 'NONE',  ( 37.80618814713140097, -15.91368208888610880, 73.13360434286903455 ) ) ;
#7332 = VECTOR ( 'NONE', #2898, 1000.000000000000000 ) ;
#7333 = CIRCLE ( 'NONE', #10634, 0.7500000000000006661 ) ;
#7334 = VECTOR ( 'NONE', #15929, 1000.000000000000227 ) ;
#7335 = ORIENTED_EDGE ( 'NONE', *, *, #13429, .F. ) ;
#7336 = CARTESIAN_POINT ( 'NONE',  ( 42.06606138205700063, 45.04446929126260102, 81.37823623207320622 ) ) ;
#7337 = DIRECTION ( 'NONE',  ( 0.000000000000000000, 0.7540134720837717852, 0.6568589528324747517 ) ) ;
#7338 = CARTESIAN_POINT ( 'NONE',  ( 36.07789103942398867, -21.41368208888610880, 70.70992431699450265 ) ) ;
#7339 = EDGE_LOOP ( 'NONE', ( #24898, #24455, #14377, #24400 ) ) ;
#7340 = SURFACE_STYLE_FILL_AREA ( #20867 ) ;
#7341 =( REPRESENTATION_RELATIONSHIP ('NONE','NONE', #17377, #10983 ) REPRESENTATION_RELATIONSHIP_WITH_TRANSFORMATION ( #8139 )SHAPE_REPRESENTATION_RELATIONSHIP( ) );
#7342 = CARTESIAN_POINT ( 'NONE',  ( 44.06606138205700063, -26.74044063519535186, 83.30501292737007191 ) ) ;
#7343 = CARTESIAN_POINT ( 'NONE',  ( 45.81606138205700063, -26.74044063519535186, 82.50501292737007475 ) ) ;
#7344 = AXIS2_PLACEMENT_3D ( 'NONE', #21061, #7533, #21188 ) ;
#7345 = LINE ( 'NONE', #21004, #19287 ) ;
#7346 = EDGE_CURVE ( 'NONE', #4607, #5873, #10416, .T. ) ;
#7347 = CARTESIAN_POINT ( 'NONE',  ( 43.31606138205700063, -22.22127907754180853, 85.30501292736998664 ) ) ;
#7348 = CARTESIAN_POINT ( 'NONE',  ( 38.37017380507018771, -21.60384086642191548, 70.24448340153875847 ) ) ;
#7349 = CARTESIAN_POINT ( 'NONE',  ( 38.26194895904383486, 0.9863179111138999922, 69.64448340153880679 ) ) ;
#7350 = AXIS2_PLACEMENT_3D ( 'NONE', #1854, #7673, #25159 ) ;
#7351 = VERTEX_POINT ( 'NONE', #1111 ) ;
#7352 = CYLINDRICAL_SURFACE ( 'NONE', #18085, 0.7500000000000006661 ) ;
#7353 = CARTESIAN_POINT ( 'NONE',  ( 40.31606138205701484, -21.38339321089542011, 27.67811916372966863 ) ) ;
#7354 = ORIENTED_EDGE ( 'NONE', *, *, #21588, .T. ) ;
#7355 = ORIENTED_EDGE ( 'NONE', *, *, #17843, .T. ) ;
#7356 = CARTESIAN_POINT ( 'NONE',  ( 36.87297107704149823, -1.903840866421906419, 70.26145752964255564 ) ) ;
#7357 = VECTOR ( 'NONE', #23174, 1000.000000000000000 ) ;
#7358 = CARTESIAN_POINT ( 'NONE',  ( 39.75915168707250302, -0.7136820888860997414, 70.26145752964252722 ) ) ;
#7359 = CARTESIAN_POINT ( 'NONE',  ( 39.73277004305198545, -12.21368208888610951, 73.23812341099225875 ) ) ;
#7360 = ORIENTED_EDGE ( 'NONE', *, *, #17415, .F. ) ;
#7361 = CARTESIAN_POINT ( 'NONE',  ( 43.06606138205700063, 41.44123852234599781, 75.30501292736987295 ) ) ;
#7362 = CARTESIAN_POINT ( 'NONE',  ( 37.89291511884479036, -4.503840866421912281, 72.49843995877331793 ) ) ;
#7363 = VECTOR ( 'NONE', #22815, 1000.000000000000000 ) ;
#7364 = EDGE_CURVE ( 'NONE', #13605, #2134, #853, .T. ) ;
#7365 = CARTESIAN_POINT ( 'NONE',  ( 43.81606138205700063, 46.92314894770293421, 79.37823623207319201 ) ) ;
#7366 = EDGE_CURVE ( 'NONE', #13966, #3395, #19439, .T. ) ;
#7367 = ORIENTED_EDGE ( 'NONE', *, *, #15799, .T. ) ;
#7368 = CARTESIAN_POINT ( 'NONE',  ( 33.66606138205698073, -6.230354416574667376, -1.331254207427787328 ) ) ;
#7369 = CARTESIAN_POINT ( 'NONE',  ( 40.31606138205700773, -19.28757846107943763, 24.56123906878952567 ) ) ;
#7370 = CARTESIAN_POINT ( 'NONE',  ( 40.26954217208372455, -6.903840866421917966, 72.86986841596736042 ) ) ;
#7371 = EDGE_CURVE ( 'NONE', #1612, #13993, #20713, .T. ) ;
#7372 = B_SPLINE_CURVE_WITH_KNOTS ( 'NONE', 3,
 ( #4142, #10072, #756, #8644, #4394, #12139, #16474, #247, #6199, #10315, #23952, #14053, #6327, #14187, #12256, #20100, #2439, #18179 ),
 .UNSPECIFIED., .F., .F.,
 ( 4, 2, 2, 2, 2, 2, 2, 2, 4 ),
 ( 0.000000000000000000, 0.1250000000000000833, 0.2500000000000001665, 0.3750000000000002220, 0.4375000000000030531, 0.5000000000000058842, 0.6250000000000059952, 0.7500000000000061062, 1.000000000000000000 ),
 .UNSPECIFIED. ) ;
#7373 = EDGE_CURVE ( 'NONE', #723, #14751, #11048, .T. ) ;
#7374 = EDGE_CURVE ( 'NONE', #24769, #21641, #22739, .T. ) ;
#7375 = CARTESIAN_POINT ( 'NONE',  ( 37.09113907096683960, -21.82847486639042955, 75.81287845682257398 ) ) ;
#7376 = AXIS2_PLACEMENT_3D ( 'NONE', #10360, #19640, #50 ) ;
#7377 = CARTESIAN_POINT ( 'NONE',  ( 32.81606138205700773, 0.9984178969752143251, 11.59873562314662010 ) ) ;
#7378 = CARTESIAN_POINT ( 'NONE',  ( 37.25202387243752611, -19.21368208888610241, 70.00779233799262613 ) ) ;
#7379 = FACE_BOUND ( 'NONE', #9287, .T. ) ;
#7380 = PLANE ( 'NONE',  #13868 ) ;
#7381 = AXIS2_PLACEMENT_3D ( 'NONE', #17259, #15188, #17521 ) ;
#7382 = VERTEX_POINT ( 'NONE', #4742 ) ;
#7383 = DIRECTION ( 'NONE',  ( 0.000000000000000000, 0.5706330172266952383, -0.8212051873014186709 ) ) ;
#7384 = EDGE_CURVE ( 'NONE', #8218, #7685, #11651, .T. ) ;
#7385 = CARTESIAN_POINT ( 'NONE',  ( 36.68196826583682935, -6.003840866421913169, 70.79240656858108593 ) ) ;
#7387 = EDGE_CURVE ( 'NONE', #203, #3058, #16579, .T. ) ;
#7386 = APPLICATION_PROTOCOL_DEFINITION ( 'draft international standard', 'automotive_design', 1998, #12622 ) ;
#7388 = PLANE ( 'NONE',  #5912 ) ;
#7389 = CIRCLE ( 'NONE', #9853, 3.000000000000002665 ) ;
#7390 = CARTESIAN_POINT ( 'NONE',  ( 37.80618814713140097, -21.91368208888610880, 73.13360434286903455 ) ) ;
#7391 = LINE ( 'NONE', #3385, #4491 ) ;
#7392 = CARTESIAN_POINT ( 'NONE',  ( 39.95015449827720744, -27.00384086642191050, 71.96809898377885872 ) ) ;
#7393 = CARTESIAN_POINT ( 'NONE',  ( 38.31606138205700063, -5.204193249396277032, 83.30501292736992980 ) ) ;
#7394 = AXIS2_PLACEMENT_3D ( 'NONE', #7477, #5036, #9174 ) ;
#7395 = ADVANCED_FACE ( 'NONE', ( #6801 ), #15034, .T. ) ;
#7396 = CARTESIAN_POINT ( 'NONE',  ( 39.75915168707250302, -18.71368208888610241, 70.26145752964251301 ) ) ;
#7397 = ORIENTED_EDGE ( 'NONE', *, *, #9353, .F. ) ;
#7398 = CARTESIAN_POINT ( 'NONE',  ( 39.64521430340305841, 1.196159133578081457, 73.30173637941821596 ) ) ;
#7399 = VERTEX_POINT ( 'NONE', #20580 ) ;
#7400 = DIRECTION ( 'NONE',  ( 2.312964634635742267E-15, -0.8967398287344627850, -0.4425581086832398592 ) ) ;
#7401 = CARTESIAN_POINT ( 'NONE',  ( 40.31606138205700773, -13.04008168869994577, 21.66778101221729713 ) ) ;
#7402 = CARTESIAN_POINT ( 'NONE',  ( 37.25260217561390874, -24.00384086642191761, 70.97781676520601479 ) ) ;
#7403 = VECTOR ( 'NONE', #22467, 1000.000000000000000 ) ;
#7404 = ORIENTED_EDGE ( 'NONE', *, *, #7665, .T. ) ;
#7405 = EDGE_LOOP ( 'NONE', ( #2181, #3021, #13770, #10345 ) ) ;
#7406 = CARTESIAN_POINT ( 'NONE',  ( 44.81606138205700063, 18.19123852234599070, 72.05501292736995822 ) ) ;
#7407 = CARTESIAN_POINT ( 'NONE',  ( 43.81606138205700063, 6.289375473607850431, 7.138843309009015314 ) ) ;
#7408 = EDGE_LOOP ( 'NONE', ( #13777, #17459, #22105, #7238 ) ) ;
#7409 = DIRECTION ( 'NONE',  ( 1.327674326049719602E-15, -0.4425581086832399147, 0.8967398287344627850 ) ) ;
#7410 = CARTESIAN_POINT ( 'NONE',  ( 38.37017380507018771, -27.60384086642191548, 69.04448340153878405 ) ) ;
#7411 = VECTOR ( 'NONE', #17471, 1000.000000000000000 ) ;
#7412 = DIRECTION ( 'NONE',  ( 1.000000000000000000, 2.490066548941357423E-15, 1.228895056384527422E-15 ) ) ;
#7413 = CARTESIAN_POINT ( 'NONE',  ( 31.81606138205700418, -33.00876147765401925, 70.30501292737011454 ) ) ;
#7414 = ORIENTED_EDGE ( 'NONE', *, *, #14443, .F. ) ;
#7415 = ORIENTED_EDGE ( 'NONE', *, *, #4994, .F. ) ;
#7416 = DIRECTION ( 'NONE',  ( 9.614242282381077875E-31, 0.7071067811865460184, 0.7071067811865489050 ) ) ;
#7417 = CARTESIAN_POINT ( 'NONE',  ( 36.49096545463212493, -3.513682088886103561, 71.43714994484035685 ) ) ;
#7418 = CARTESIAN_POINT ( 'NONE',  ( 36.80608444377002542, -26.30384086642191477, 72.40698646996131060 ) ) ;
#7419 =( NAMED_UNIT ( * ) PLANE_ANGLE_UNIT ( ) SI_UNIT ( $, .RADIAN. ) );
#7420 = CARTESIAN_POINT ( 'NONE',  ( 46.81606138205695089, 5.290470704224636833, -0.3848988112044732235 ) ) ;
#7421 = ORIENTED_EDGE ( 'NONE', *, *, #23881, .T. ) ;
#7422 = CARTESIAN_POINT ( 'NONE',  ( 45.06606138205707879, -39.09901169483119077, 63.57464975149194686 ) ) ;
#7423 = AXIS2_PLACEMENT_3D ( 'NONE', #24972, #14354, #20529 ) ;
#7424 = CARTESIAN_POINT ( 'NONE',  ( 43.31606138205700063, -33.36512788127016904, 60.17493381834628252 ) ) ;
#7425 = DIRECTION ( 'NONE',  ( 0.000000000000000000, -1.000000000000000000, 2.999999999999999839E-15 ) ) ;
#7426 = EDGE_LOOP ( 'NONE', ( #17029, #16678, #16634, #3323, #7414, #24320 ) ) ;
#7427 = CARTESIAN_POINT ( 'NONE',  ( 38.31606138205700063, 40.69123852234599781, 71.30501292737000085 ) ) ;
#7428 = ORIENTED_EDGE ( 'NONE', *, *, #12228, .T. ) ;
#7429 = EDGE_LOOP ( 'NONE', ( #8161, #10821, #15289, #16289 ) ) ;
#7430 = CARTESIAN_POINT ( 'NONE',  ( 43.31606138205700063, -0.03546393544221274063, 20.62209909563275900 ) ) ;
#7431 = CARTESIAN_POINT ( 'NONE',  ( 39.51027997493896748, -14.51368208888610134, 71.32335560751960202 ) ) ;
#7432 = CARTESIAN_POINT ( 'NONE',  ( 39.41296390513587511, -12.41368208888609992, 71.67976084211551324 ) ) ;
#7433 = ORIENTED_EDGE ( 'NONE', *, *, #21800, .F. ) ;
#7434 = ORIENTED_EDGE ( 'NONE', *, *, #7051, .T. ) ;
#7435 = CARTESIAN_POINT ( 'NONE',  ( 29.71606138205696368, 0.06621141594066179414, 0.03267658921015577367 ) ) ;
#7436 = CARTESIAN_POINT ( 'NONE',  ( 30.81606138205697221, -29.47337283097074234, 44.07055847651731995 ) ) ;
#7437 = CARTESIAN_POINT ( 'NONE',  ( 36.80608444377001831, -26.30384086642191477, 72.40698646996133903 ) ) ;
#7438 = AXIS2_PLACEMENT_3D ( 'NONE', #8508, #22028, #8255 ) ;
#7439 = DIRECTION ( 'NONE',  ( 0.000000000000000000, -1.000000000000000000, 6.123233995736769734E-17 ) ) ;
#7440 = CARTESIAN_POINT ( 'NONE',  ( 39.31564783533280405, -20.31368208888610027, 72.03616607671141026 ) ) ;
#7441 = VECTOR ( 'NONE', #20087, 1000.000000000000000 ) ;
#7442 = ORIENTED_EDGE ( 'NONE', *, *, #17056, .F. ) ;
#7443 = FACE_OUTER_BOUND ( 'NONE', #25009, .T. ) ;
#7444 = CARTESIAN_POINT ( 'NONE',  ( 30.81606138205700418, -26.97987052895604876, 80.55501292737007191 ) ) ;
#7445 = DIRECTION ( 'NONE',  ( 0.000000000000000000, -0.7516416929448823669, -0.6595716529892345914 ) ) ;
#7446 = CARTESIAN_POINT ( 'NONE',  ( 38.83610899671118943, -5.265426583881079203, 82.80485556514678080 ) ) ;
#7447 = PLANE ( 'NONE',  #24568 ) ;
#7448 = EDGE_CURVE ( 'NONE', #24976, #19369, #3394, .T. ) ;
#7449 = CARTESIAN_POINT ( 'NONE',  ( 32.81606138205700773, 41.44123852234599070, 73.05501292736987295 ) ) ;
#7450 = EDGE_CURVE ( 'NONE', #7462, #7938, #20840, .T. ) ;
#7451 = ORIENTED_EDGE ( 'NONE', *, *, #11713, .F. ) ;
#7452 = AXIS2_PLACEMENT_3D ( 'NONE', #10767, #14368, #18121 ) ;
#7453 = PLANE ( 'NONE',  #15618 ) ;
#7454 = CARTESIAN_POINT ( 'NONE',  ( 30.81606138205706813, -35.90867894478445521, 74.07034463014319670 ) ) ;
#7455 = ORIENTED_EDGE ( 'NONE', *, *, #15389, .F. ) ;
#7456 = ORIENTED_EDGE ( 'NONE', *, *, #18801, .T. ) ;
#7457 = AXIS2_PLACEMENT_3D ( 'NONE', #305, #20289, #57 ) ;
#7458 = CARTESIAN_POINT ( 'NONE',  ( 36.11133435605973574, -12.00384086642191583, 70.60699637195608602 ) ) ;
#7459 = CARTESIAN_POINT ( 'NONE',  ( 40.64099152588523367, -8.607181138186998481, 78.30501292736998664 ) ) ;
#7460 = CARTESIAN_POINT ( 'NONE',  ( 37.25202387243752611, -13.21368208888610063, 70.00779233799262613 ) ) ;
#7461 = PRESENTATION_STYLE_ASSIGNMENT (( #11725 ) ) ;
#7462 = VERTEX_POINT ( 'NONE', #22763 ) ;
#7463 = CARTESIAN_POINT ( 'NONE',  ( 33.48998873999627079, 2.908502444426765532, 6.098666494912968972 ) ) ;
#7464 = DIRECTION ( 'NONE',  ( -1.000000000000000000, -2.999999999999999839E-15, 0.000000000000000000 ) ) ;
#7465 = EDGE_CURVE ( 'NONE', #9234, #1958, #9990, .T. ) ;
#7466 = CARTESIAN_POINT ( 'NONE',  ( 36.36258059203031934, -23.71368208888610951, 72.86986841596734621 ) ) ;
#7467 = ORIENTED_EDGE ( 'NONE', *, *, #19005, .F. ) ;
#7468 = FACE_OUTER_BOUND ( 'NONE', #2125, .T. ) ;
#7469 = LINE ( 'NONE', #3592, #6967 ) ;
#7470 = FACE_OUTER_BOUND ( 'NONE', #7157, .T. ) ;
#7471 = CARTESIAN_POINT ( 'NONE',  ( 29.81606138205707168, -37.70325315460882365, 65.37863370302704880 ) ) ;
#7472 =( GEOMETRIC_REPRESENTATION_CONTEXT ( 3 ) GLOBAL_UNCERTAINTY_ASSIGNED_CONTEXT ( ( #12580 ) ) GLOBAL_UNIT_ASSIGNED_CONTEXT ( ( #1309, #19101, #1439 ) ) REPRESENTATION_CONTEXT ( 'NONE', 'WORKASPACE' ) );
#7473 = DIRECTION ( 'NONE',  ( 0.000000000000000000, 0.4425581086832400812, -0.8967398287344626739 ) ) ;
#7474 = CARTESIAN_POINT ( 'NONE',  ( 37.60469502381300799, -10.40384086642191086, 72.26730301774236409 ) ) ;
#7475 = CARTESIAN_POINT ( 'NONE',  ( 39.98359781491296161, 1.586317911113896528, 71.86517103874049894 ) ) ;
#7476 = ORIENTED_EDGE ( 'NONE', *, *, #14433, .T. ) ;
#7477 = CARTESIAN_POINT ( 'NONE',  ( 36.31606138205700063, -5.204193249396356968, 72.80501292736992980 ) ) ;
#7478 = CYLINDRICAL_SURFACE ( 'NONE', #13183, 0.4999999999999982792 ) ;
#7479 = ORIENTED_EDGE ( 'NONE', *, *, #17781, .T. ) ;
#7480 = ORIENTED_EDGE ( 'NONE', *, *, #24326, .T. ) ;
#7481 = CARTESIAN_POINT ( 'NONE',  ( 39.12911128074872380, -27.50384086642191406, 69.06206559358663810 ) ) ;
#7482 = CARTESIAN_POINT ( 'NONE',  ( 39.95015449827720744, 1.386317911113894130, 70.79240656858108593 ) ) ;
#7483 = CARTESIAN_POINT ( 'NONE',  ( 38.37017380507020192, -2.013682088886109334, 73.71602215082116061 ) ) ;
#7484 = AXIS2_PLACEMENT_3D ( 'NONE', #20969, #1379, #13620 ) ;
#7485 = ORIENTED_EDGE ( 'NONE', *, *, #21470, .T. ) ;
#7486 = DIRECTION ( 'NONE',  ( 7.386467098469070069E-45, -1.000000000000000000, 3.000000000000004177E-15 ) ) ;
#7487 = AXIS2_PLACEMENT_3D ( 'NONE', #13512, #5910, #4108 ) ;
#7488 = CARTESIAN_POINT ( 'NONE',  ( 37.60469502381300799, -4.403840866421911748, 72.26730301774236409 ) ) ;
#7489 = LINE ( 'NONE', #10313, #15948 ) ;
#7490 = ORIENTED_EDGE ( 'NONE', *, *, #18033, .T. ) ;
#7491 = CARTESIAN_POINT ( 'NONE',  ( 31.81606138205700418, 41.44123852234596939, 66.30501292736988717 ) ) ;
#7492 = CARTESIAN_POINT ( 'NONE',  ( 30.81606138205700418, -30.95005513552129983, 81.04249030099066431 ) ) ;
#7493 = EDGE_CURVE ( 'NONE', #16518, #23360, #24428, .T. ) ;
#7494 = AXIS2_PLACEMENT_3D ( 'NONE', #6792, #24671, #3301 ) ;
#7495 = CARTESIAN_POINT ( 'NONE',  ( 40.77203464402485622, -11.10384086642191193, 71.43714994484034264 ) ) ;
#7496 = FACE_OUTER_BOUND ( 'NONE', #5774, .T. ) ;
#7497 = DIRECTION ( 'NONE',  ( 0.000000000000000000, -0.5706330172266952383, 0.8212051873014186709 ) ) ;
#7498 = CARTESIAN_POINT ( 'NONE',  ( 40.14115730948191185, -14.51368208888610667, 71.32335560751960202 ) ) ;
#7499 = FACE_OUTER_BOUND ( 'NONE', #8229, .T. ) ;
#7500 = DIRECTION ( 'NONE',  ( 0.000000000000000000, 1.000000000000000000, 0.000000000000000000 ) ) ;
#7501 = ORIENTED_EDGE ( 'NONE', *, *, #6272, .T. ) ;
#7502 = FACE_OUTER_BOUND ( 'NONE', #692, .T. ) ;
#7503 = CARTESIAN_POINT ( 'NONE',  ( 39.82603832034401137, -5.303840866421906775, 70.35351908239860563 ) ) ;
#7504 = SHAPE_DEFINITION_REPRESENTATION ( #5597, #10983 ) ;
#7505 = AXIS2_PLACEMENT_3D ( 'NONE', #10802, #24817, #10683 ) ;
#7506 = CARTESIAN_POINT ( 'NONE',  ( 33.42807400205546742, 3.632122393466618249, 6.321668986087207287 ) ) ;
#7507 = ADVANCED_FACE ( 'NONE', ( #4863, #12991 ), #10927, .F. ) ;
#7508 = CARTESIAN_POINT ( 'NONE',  ( 39.82603832034400426, -16.31368208888610738, 72.40698646996133903 ) ) ;
#7509 = EDGE_CURVE ( 'NONE', #16850, #10286, #24299, .T. ) ;
#7510 = DIRECTION ( 'NONE',  ( -1.000000000000000000, 0.000000000000000000, 0.000000000000000000 ) ) ;
#7511 = AXIS2_PLACEMENT_3D ( 'NONE', #19787, #19534, #11696 ) ;
#7512 = EDGE_CURVE ( 'NONE', #16332, #6994, #918, .T. ) ;
#7513 = EDGE_CURVE ( 'NONE', #1156, #13201, #84, .T. ) ;
#7514 = CARTESIAN_POINT ( 'NONE',  ( 39.38009889167648936, -19.40384086642190908, 70.00779233799262613 ) ) ;
#7515 = EDGE_CURVE ( 'NONE', #22306, #24213, #18775, .T. ) ;
#7516 = LINE ( 'NONE', #13439, #18389 ) ;
#7517 = VECTOR ( 'NONE', #7728, 1000.000000000000000 ) ;
#7518 = CARTESIAN_POINT ( 'NONE',  ( 37.80618814713140097, -15.91368208888610880, 73.13360434286903455 ) ) ;
#7519 = EDGE_LOOP ( 'NONE', ( #15686, #17082, #12946, #24007 ) ) ;
#7520 = CARTESIAN_POINT ( 'NONE',  ( 40.77203464402485622, -24.51368208888610667, 71.32335560751960202 ) ) ;
#7521 = VECTOR ( 'NONE', #18282, 1000.000000000000114 ) ;
#7522 = ORIENTED_EDGE ( 'NONE', *, *, #21655, .F. ) ;
#7523 = CARTESIAN_POINT ( 'NONE',  ( 35.64099152588522657, -1.357181138186998925, 80.05501292737000085 ) ) ;
#7524 = FACE_OUTER_BOUND ( 'NONE', #20441, .T. ) ;
#7525 = SHAPE_REPRESENTATION ( 'Staple Magazine', ( #2000 ), #6773 ) ;
#7526 = CARTESIAN_POINT ( 'NONE',  ( 39.02742774030101458, -23.40384086642191264, 70.49320253461759478 ) ) ;
#7527 = ORIENTED_EDGE ( 'NONE', *, *, #8713, .F. ) ;
#7528 = EDGE_LOOP ( 'NONE', ( #8544, #19798, #1789, #17372 ) ) ;
#7529 = DIRECTION ( 'NONE',  ( -1.000000000000000000, -1.052872940142565459E-15, -1.848188032574765003E-17 ) ) ;
#7530 = DIRECTION ( 'NONE',  ( 1.000000000000000000, 0.000000000000000000, 0.000000000000000000 ) ) ;
#7531 = ORIENTED_EDGE ( 'NONE', *, *, #1692, .F. ) ;
#7532 = ADVANCED_FACE ( 'NONE', ( #24545 ), #6927, .F. ) ;
#7534 = AXIS2_PLACEMENT_3D ( 'NONE', #8550, #2004, #12426 ) ;
#7533 = DIRECTION ( 'NONE',  ( 1.000000000000000000, 0.000000000000000000, 0.000000000000000000 ) ) ;
#7535 = CARTESIAN_POINT ( 'NONE',  ( 38.26194895904384907, -0.6038408664219147015, 73.11602215082118050 ) ) ;
#7536 = EDGE_CURVE ( 'NONE', #11745, #4935, #5854, .T. ) ;
#7537 = VECTOR ( 'NONE', #176, 1000.000000000000227 ) ;
#7538 = CARTESIAN_POINT ( 'NONE',  ( 39.81606138205700063, -7.086900875803856970, 56.51273394326043586 ) ) ;
#7539 = AXIS2_PLACEMENT_3D ( 'NONE', #17833, #13830, #5465 ) ;
#7540 = LINE ( 'NONE', #9609, #8575 ) ;
#7541 = EDGE_LOOP ( 'NONE', ( #14798, #2150, #11777, #23009 ) ) ;
#7542 = VERTEX_POINT ( 'NONE', #17354 ) ;
#7543 = LINE ( 'NONE', #15134, #19897 ) ;
#7544 = CARTESIAN_POINT ( 'NONE',  ( 40.81606138205700773, 41.44123852234599781, 75.30501292736988717 ) ) ;
#7545 = AXIS2_PLACEMENT_3D ( 'NONE', #2265, #10141, #14133 ) ;
#7546 = CARTESIAN_POINT ( 'NONE',  ( 37.80618814713138676, -27.70384086642190624, 69.62690120949091011 ) ) ;
#7547 = CARTESIAN_POINT ( 'NONE',  ( 33.31606138205700773, -5.204193249396277032, 83.30501292736992980 ) ) ;
#7548 = ORIENTED_EDGE ( 'NONE', *, *, #22457, .F. ) ;
#7549 = LINE ( 'NONE', #15400, #3623 ) ;
#7550 = AXIS2_PLACEMENT_3D ( 'NONE', #17187, #15245, #25011 ) ;
#7551 = AXIS2_PLACEMENT_3D ( 'NONE', #19602, #2326, #11892 ) ;
#7552 = PLANE ( 'NONE',  #11098 ) ;
#7553 = CYLINDRICAL_SURFACE ( 'NONE', #21266, 1.000000000000000888 ) ;
#7554 = EDGE_CURVE ( 'NONE', #13632, #12758, #14496, .T. ) ;
#7555 = CARTESIAN_POINT ( 'NONE',  ( 38.37017380507018771, -5.603840866421911926, 70.24448340153877268 ) ) ;
#7556 = ADVANCED_FACE ( 'NONE', ( #21471 ), #3736, .T. ) ;
#7557 = ORIENTED_EDGE ( 'NONE', *, *, #6571, .T. ) ;
#7558 = AXIS2_PLACEMENT_3D ( 'NONE', #12011, #6450, #503 ) ;
#7559 = CYLINDRICAL_SURFACE ( 'NONE', #1652, 0.5000000000000004441 ) ;
#7560 = ORIENTED_EDGE ( 'NONE', *, *, #10186, .F. ) ;
#7561 = ORIENTED_EDGE ( 'NONE', *, *, #16350, .T. ) ;
#7562 = CARTESIAN_POINT ( 'NONE',  ( 40.31606138205700773, 43.19123852234596939, 65.30501292736988717 ) ) ;
#7563 = CARTESIAN_POINT ( 'NONE',  ( 37.21915885897815457, -11.41368208888610170, 71.08074471024443142 ) ) ;
#7564 = CARTESIAN_POINT ( 'NONE',  ( 39.41296390513587511, -10.41368208888610170, 71.67976084211552745 ) ) ;
#7565 = ORIENTED_EDGE ( 'NONE', *, *, #10147, .F. ) ;
#7566 = VECTOR ( 'NONE', #14227, 1000.000000000000000 ) ;
#7567 = ORIENTED_EDGE ( 'NONE', *, *, #10707, .T. ) ;
#7568 = DIRECTION ( 'NONE',  ( 0.000000000000000000, 0.7540134720837717852, 0.6568589528324746407 ) ) ;
#7569 = CARTESIAN_POINT ( 'NONE',  ( 33.31606138205700773, -33.60910547091194900, 60.61426200347987248 ) ) ;
#7570 = CARTESIAN_POINT ( 'NONE',  ( 44.81606138205700063, -30.95005513552129983, 81.04249030099066431 ) ) ;
#7571 = CARTESIAN_POINT ( 'NONE',  ( 37.33957961208645315, -19.80384086642191122, 69.94417936956672577 ) ) ;
#7572 = CARTESIAN_POINT ( 'NONE',  ( 45.06606138205707879, -38.42645682328033985, 63.90656833300437256 ) ) ;
#7573 = B_SPLINE_CURVE_WITH_KNOTS ( 'NONE', 3,
 ( #13810, #14201, #10327, #4405, #4018, #20116, #3894, #2207, #21548, #18189 ),
 .UNSPECIFIED., .F., .F.,
 ( 4, 3, 3, 4 ),
 ( 2.611104600503255186E-18, 0.0001276540846395581876, 0.0002420623083067835056, 0.0003579128776106695184 ),
 .UNSPECIFIED. ) ;
#7574 = CARTESIAN_POINT ( 'NONE',  ( 37.12184278917507640, -15.51368208888610312, 71.43714994484034264 ) ) ;
#7575 = VERTEX_POINT ( 'NONE', #1875 ) ;
#7576 = VECTOR ( 'NONE', #18758, 1000.000000000000000 ) ;
#7577 = ORIENTED_EDGE ( 'NONE', *, *, #10668, .T. ) ;
#7578 = ORIENTED_EDGE ( 'NONE', *, *, #7846, .F. ) ;
#7579 = DIRECTION ( 'NONE',  ( 1.000000000000000000, 1.000000000000000078E-15, 0.000000000000000000 ) ) ;
#7580 = EDGE_CURVE ( 'NONE', #18044, #9433, #25053, .T. ) ;
#7581 = AXIS2_PLACEMENT_3D ( 'NONE', #2035, #5915, #9916 ) ;
#7582 = FACE_BOUND ( 'NONE', #15241, .T. ) ;
#7583 = LINE ( 'NONE', #19411, #24340 ) ;
#7584 = CARTESIAN_POINT ( 'NONE',  ( 40.31606138205700773, -7.073990261058225926, 83.13804008194063044 ) ) ;
#7585 = CARTESIAN_POINT ( 'NONE',  ( 31.81606138205700418, 39.19123852234599070, 72.05501292736988717 ) ) ;
#7586 = CARTESIAN_POINT ( 'NONE',  ( 38.31606138205700063, -6.758471399387619094, 56.13572720721855092 ) ) ;
#7587 = ORIENTED_EDGE ( 'NONE', *, *, #1235, .T. ) ;
#7588 =( GEOMETRIC_REPRESENTATION_CONTEXT ( 3 ) GLOBAL_UNCERTAINTY_ASSIGNED_CONTEXT ( ( #20090 ) ) GLOBAL_UNIT_ASSIGNED_CONTEXT ( ( #6048, #17779, #12118 ) ) REPRESENTATION_CONTEXT ( 'NONE', 'WORKASPACE' ) );
#7589 = DIRECTION ( 'NONE',  ( -1.000000000000000000, -2.751104698760144965E-15, 1.228345504986737969E-16 ) ) ;
#7590 = ORIENTED_EDGE ( 'NONE', *, *, #3104, .T. ) ;
#7591 = ORIENTED_EDGE ( 'NONE', *, *, #20647, .F. ) ;
#7592 = AXIS2_PLACEMENT_3D ( 'NONE', #9094, #9224, #3008 ) ;
#7593 = CARTESIAN_POINT ( 'NONE',  ( 40.33642880535521869, -11.30384086642191299, 69.98269868914867686 ) ) ;
#7594 = CIRCLE ( 'NONE', #3888, 1.000000000000000888 ) ;
#7595 = DIRECTION ( 'NONE',  ( -1.786044098272412642E-16, -0.4425581086832399702, 0.8967398287344628960 ) ) ;
#7596 = CARTESIAN_POINT ( 'NONE',  ( 37.25202387243752611, -17.21368208888610241, 70.00779233799262613 ) ) ;
#7597 = ORIENTED_EDGE ( 'NONE', *, *, #24233, .T. ) ;
#7598 = CARTESIAN_POINT ( 'NONE',  ( 38.41621794735363693, -35.10729675983900222, 84.30501292737010033 ) ) ;
#7599 = CARTESIAN_POINT ( 'NONE',  ( 35.81606138205700063, -31.05876147765399864, 75.30501292737010033 ) ) ;
#7600 = CARTESIAN_POINT ( 'NONE',  ( 38.26194895904383486, -19.01368208888609956, 69.04448340153878405 ) ) ;
#7601 = ORIENTED_EDGE ( 'NONE', *, *, #19451, .F. ) ;
#7602 = EDGE_CURVE ( 'NONE', #10132, #19839, #11437, .T. ) ;
#7603 = LINE ( 'NONE', #5539, #9039 ) ;
#7604 = EDGE_CURVE ( 'NONE', #2759, #21678, #3443, .T. ) ;
#7605 = DIRECTION ( 'NONE',  ( 0.000000000000000000, -0.6568589528324746407, 0.7540134720837717852 ) ) ;
#7606 = CARTESIAN_POINT ( 'NONE',  ( 40.31606138205700773, -31.05876147765400574, 73.55501292737010033 ) ) ;
#7607 = EDGE_CURVE ( 'NONE', #4892, #2928, #5886, .T. ) ;
#7608 = FACE_OUTER_BOUND ( 'NONE', #24255, .T. ) ;
#7609 = AXIS2_PLACEMENT_3D ( 'NONE', #5059, #3240, #3117 ) ;
#7610 = CARTESIAN_POINT ( 'NONE',  ( 36.72255525790973252, -5.988568098966074338, 83.27624199006054084 ) ) ;
#7611 = CARTESIAN_POINT ( 'NONE',  ( 38.00113996487112189, -11.70384086642191335, 70.22690120949091863 ) ) ;
#7612 = CARTESIAN_POINT ( 'NONE',  ( 38.93987200065208754, -28.81368208888610383, 70.42958956619166599 ) ) ;
#7613 = ORIENTED_EDGE ( 'NONE', *, *, #11384, .T. ) ;
#7614 = DIRECTION ( 'NONE',  ( -1.000000000000000000, -3.046345864243081103E-15, -1.366653866685768465E-16 ) ) ;
#7615 = B_SPLINE_CURVE_WITH_KNOTS ( 'NONE', 3,
 ( #17749, #81, #9766, #3827 ),
 .UNSPECIFIED., .F., .F.,
 ( 4, 4 ),
 ( 0.000000000000000000, 1.000000000000000000 ),
 .UNSPECIFIED. ) ;
#7616 = CARTESIAN_POINT ( 'NONE',  ( 42.96606138205698500, -6.570990706613058840, -2.335727660491067503 ) ) ;
#7617 = ORIENTED_EDGE ( 'NONE', *, *, #24822, .F. ) ;
#7618 = ORIENTED_EDGE ( 'NONE', *, *, #23820, .T. ) ;
#7619 = CARTESIAN_POINT ( 'NONE',  ( 39.73277004305197124, -27.40384086642191619, 69.52238214136765748 ) ) ;
#7620 = CARTESIAN_POINT ( 'NONE',  ( 37.21915885897815457, -27.41368208888609814, 71.08074471024441721 ) ) ;
#7621 = CARTESIAN_POINT ( 'NONE',  ( 38.26194895904383486, -3.013682088886100008, 69.04448340153881247 ) ) ;
#7622 = ORIENTED_EDGE ( 'NONE', *, *, #7210, .F. ) ;
#7623 = CARTESIAN_POINT ( 'NONE',  ( 43.23147868389327897, 41.43850569188389699, 79.87823623207322044 ) ) ;
#7624 = CARTESIAN_POINT ( 'NONE',  ( 38.37017380507018771, -5.603840866421911926, 70.24448340153877268 ) ) ;
#7625 = VECTOR ( 'NONE', #8653, 1000.000000000000000 ) ;
#7626 = CARTESIAN_POINT ( 'NONE',  ( 36.31606138205702194, -20.30191568716149320, 23.22716926412510219 ) ) ;
#7627 = VERTEX_POINT ( 'NONE', #24925 ) ;
#7628 = DIRECTION ( 'NONE',  ( 1.000000000000000000, 2.999999999999999839E-15, 0.000000000000000000 ) ) ;
#7629 = PLANE ( 'NONE',  #15355 ) ;
#7630 = CARTESIAN_POINT ( 'NONE',  ( 36.98690846071097127, -7.803840866421912104, 69.45876917294177133 ) ) ;
#7631 = LINE ( 'NONE', #9569, #8234 ) ;
#7632 =( LENGTH_UNIT ( ) NAMED_UNIT ( * ) SI_UNIT ( .MILLI., .METRE. ) );
#7633 = CARTESIAN_POINT ( 'NONE',  ( 38.82593461698262871, -12.91368208888610347, 69.62690120949091011 ) ) ;
#7634 = CARTESIAN_POINT ( 'NONE',  ( 34.06606138205700773, 2.740850673309605412, 6.112030963703427133 ) ) ;
#7635 = DIRECTION ( 'NONE',  ( 0.000000000000000000, 1.000000000000000000, -2.999999999999999839E-15 ) ) ;
#7636 = EDGE_LOOP ( 'NONE', ( #11742, #13818, #19811, #23056 ) ) ;
#7637 = CARTESIAN_POINT ( 'NONE',  ( 33.31606138205700773, 7.043113989679085307, 66.83274420321491505 ) ) ;
#7638 = CARTESIAN_POINT ( 'NONE',  ( 37.25202387243754032, -4.403840866421916189, 72.75271321436733274 ) ) ;
#7639 = VECTOR ( 'NONE', #11219, 1000.000000000000227 ) ;
#7640 = APPLICATION_PROTOCOL_DEFINITION ( 'draft international standard', 'automotive_design', 1998, #14412 ) ;
#7641 = CARTESIAN_POINT ( 'NONE',  ( 33.23058527440274190, 3.113468987225101348, 6.136968036621309963 ) ) ;
#7642 = CARTESIAN_POINT ( 'NONE',  ( 39.38009889167650357, -18.21368208888610951, 72.75271321436731853 ) ) ;
#7643 = LINE ( 'NONE', #23335, #24205 ) ;
#7644 = EDGE_CURVE ( 'NONE', #2290, #10641, #5379, .T. ) ;
#7645 = CARTESIAN_POINT ( 'NONE',  ( 39.82603832034400426, -19.30384086642190056, 70.35351908239857721 ) ) ;
#7646 = CARTESIAN_POINT ( 'NONE',  ( 36.51585873400316018, -6.323645680884924403, 83.25095475337030848 ) ) ;
#7647 = CARTESIAN_POINT ( 'NONE',  ( 36.87297107704152666, -15.71368208888610596, 72.49904802271740323 ) ) ;
#7648 = VERTEX_POINT ( 'NONE', #9760 ) ;
#7649 = CARTESIAN_POINT ( 'NONE',  ( 40.77203464402485622, -20.51368208888610667, 71.32335560751960202 ) ) ;
#7650 = EDGE_LOOP ( 'NONE', ( #11210, #5427, #18516, #21243 ) ) ;
#7651 = CARTESIAN_POINT ( 'NONE',  ( 43.31606138205700063, -26.06829118875199924, 75.30501292736998664 ) ) ;
#7652 = LINE ( 'NONE', #19492, #12492 ) ;
#7653 = CARTESIAN_POINT ( 'NONE',  ( 37.69225076346193504, -21.80384086642191122, 70.42958956619168021 ) ) ;
#7654 = ORIENTED_EDGE ( 'NONE', *, *, #14473, .F. ) ;
#7655 = ORIENTED_EDGE ( 'NONE', *, *, #24182, .F. ) ;
#7656 = CARTESIAN_POINT ( 'NONE',  ( 39.59167754530926686, -28.73258042513078436, 70.34536827862072528 ) ) ;
#7657 = DIRECTION ( 'NONE',  ( -1.000000000000000000, 0.000000000000000000, 2.507072128559814651E-16 ) ) ;
#7658 = CARTESIAN_POINT ( 'NONE',  ( 36.31606138205700063, 43.19123852234599781, 75.30501292736987295 ) ) ;
#7659 = CARTESIAN_POINT ( 'NONE',  ( 40.26954217208372455, -28.90384086642191619, 72.86986841596730358 ) ) ;
#7660 = EDGE_CURVE ( 'NONE', #18894, #22752, #23015, .T. ) ;
#7661 = EDGE_CURVE ( 'NONE', #5882, #12862, #21096, .T. ) ;
#7662 = PRODUCT ( 'Pusher Guide Rod', 'Pusher Guide Rod', '', ( #13059 ) ) ;
#7663 = CARTESIAN_POINT ( 'NONE',  ( 31.81606138205700418, 1.441238522345979600, 68.80501292737000085 ) ) ;
#7664 = EDGE_LOOP ( 'NONE', ( #8322, #15922, #6018, #9546 ) ) ;
#7665 = EDGE_CURVE ( 'NONE', #11230, #20225, #3380, .T. ) ;
#7666 = ORIENTED_EDGE ( 'NONE', *, *, #7061, .F. ) ;
#7667 = LINE ( 'NONE', #25153, #4663 ) ;
#7668 = LINE ( 'NONE', #23491, #11822 ) ;
#7669 = CARTESIAN_POINT ( 'NONE',  ( 38.93415946300897446, -27.50384086642190340, 69.66206559358661821 ) ) ;
#7670 = SURFACE_STYLE_FILL_AREA ( #5482 ) ;
#7671 = LINE ( 'NONE', #17208, #12065 ) ;
#7672 = ORIENTED_EDGE ( 'NONE', *, *, #7843, .T. ) ;
#7673 = DIRECTION ( 'NONE',  ( -1.734723475976804876E-16, -3.469446951953610245E-15, -1.000000000000000000 ) ) ;
#7674 = EDGE_CURVE ( 'NONE', #1739, #24795, #23136, .T. ) ;
#7675 = CARTESIAN_POINT ( 'NONE',  ( 42.96606138205698500, -7.345467396808729177, -0.7664329602057526891 ) ) ;
#7676 = DIRECTION ( 'NONE',  ( -1.327674326049719602E-15, 0.4425581086832399147, -0.8967398287344627850 ) ) ;
#7677 = CARTESIAN_POINT ( 'NONE',  ( 39.51027997493896748, -9.103840866421911926, 71.43714994484034264 ) ) ;
#7678 = ORIENTED_EDGE ( 'NONE', *, *, #1840, .T. ) ;
#7679 = DIRECTION ( 'NONE',  ( -1.734723475976809806E-16, 0.000000000000000000, -1.000000000000000000 ) ) ;
#7680 = ORIENTED_EDGE ( 'NONE', *, *, #21393, .F. ) ;
#7681 = ORIENTED_EDGE ( 'NONE', *, *, #18303, .F. ) ;
#7682 = DIRECTION ( 'NONE',  ( 1.000000000000000000, 0.000000000000000000, 0.000000000000000000 ) ) ;
#7683 = CARTESIAN_POINT ( 'NONE',  ( 39.02742774030102879, -10.21368208888610241, 72.26730301774236409 ) ) ;
#7684 = CARTESIAN_POINT ( 'NONE',  ( 37.21915885897815457, -13.41368208888610170, 71.08074471024443142 ) ) ;
#7685 = VERTEX_POINT ( 'NONE', #15421 ) ;
#7686 = VERTEX_POINT ( 'NONE', #23267 ) ;
#7687 = CARTESIAN_POINT ( 'NONE',  ( 43.31606138205700773, -23.16691978223481385, 31.29201591705069063 ) ) ;
#7688 = CARTESIAN_POINT ( 'NONE',  ( 32.81606138205700773, -33.60910547091194900, 60.61426200347987248 ) ) ;
#7689 = CARTESIAN_POINT ( 'NONE',  ( 40.31606138205700773, 37.44123852234599781, 74.30501292736988717 ) ) ;
#7690 = CARTESIAN_POINT ( 'NONE',  ( 37.80618814713138676, -15.70384086642191157, 69.62690120949091011 ) ) ;
#7691 = ADVANCED_FACE ( 'NONE', ( #1742 ), #9641, .F. ) ;
#7692 = EDGE_CURVE ( 'NONE', #5392, #10132, #8078, .T. ) ;
#7693 = CARTESIAN_POINT ( 'NONE',  ( 36.31606138205700063, 6.191238522346988127, 65.30501292736998664 ) ) ;
#7694 = CARTESIAN_POINT ( 'NONE',  ( 37.69225076346193504, -21.81368208888610027, 72.33091598616826445 ) ) ;
#7695 = EDGE_CURVE ( 'NONE', #868, #9234, #878, .T. ) ;
#7696 = EDGE_CURVE ( 'NONE', #2503, #5245, #21851, .T. ) ;
#7697 = ADVANCED_FACE ( 'NONE', ( #4794 ), #6140, .F. ) ;
#7698 = ORIENTED_EDGE ( 'NONE', *, *, #9198, .T. ) ;
#7699 = CARTESIAN_POINT ( 'NONE',  ( 38.31606138205700063, -5.204193249396277032, 83.30501292736992980 ) ) ;
#7700 = CARTESIAN_POINT ( 'NONE',  ( 38.93415946300898867, -14.11368208888610809, 73.09843995877329803 ) ) ;
#7701 = CARTESIAN_POINT ( 'NONE',  ( 32.56606138205700773, 40.39281886181299797, 82.55501292736983032 ) ) ;
#7702 = CARTESIAN_POINT ( 'NONE',  ( 40.56606138205695089, 4.312150376739281477, 4.986822452676363149 ) ) ;
#7703 = CARTESIAN_POINT ( 'NONE',  ( 40.11623881305710881, -6.323557511870723680, 83.25096693106735302 ) ) ;
#7704 = LINE ( 'NONE', #5769, #25422 ) ;
#7705 = EDGE_CURVE ( 'NONE', #12562, #16296, #72, .T. ) ;
#7706 = AXIS2_PLACEMENT_3D ( 'NONE', #24909, #7676, #21453 ) ;
#7707 = CYLINDRICAL_SURFACE ( 'NONE', #15592, 1.550000000000002709 ) ;
#7708 = CIRCLE ( 'NONE', #1910, 1.500000000000001332 ) ;
#7709 = CIRCLE ( 'NONE', #22100, 1.000000000000000888 ) ;
#7710 = ORIENTED_EDGE ( 'NONE', *, *, #17518, .T. ) ;
#7711 = DIRECTION ( 'NONE',  ( -2.048868001712899108E-15, 0.6595716529892353686, -0.7516416929448815898 ) ) ;
#7712 = VERTEX_POINT ( 'NONE', #17874 ) ;
#7713 = EDGE_LOOP ( 'NONE', ( #3025, #11136, #23372, #25200 ) ) ;
#7714 = CARTESIAN_POINT ( 'NONE',  ( 37.50301148336529877, -10.50384086642191761, 73.69843995877330656 ) ) ;
#7715 = ORIENTED_EDGE ( 'NONE', *, *, #23324, .T. ) ;
#7716 = EDGE_CURVE ( 'NONE', #7176, #13053, #21726, .T. ) ;
#7717 = LINE ( 'NONE', #9909, #12848 ) ;
#7718 = CARTESIAN_POINT ( 'NONE',  ( 37.33957961208646736, -17.81368208888611093, 72.81632618279321889 ) ) ;
#7719 = ORIENTED_EDGE ( 'NONE', *, *, #17127, .T. ) ;
#7720 = CARTESIAN_POINT ( 'NONE',  ( 33.35563295957085472, 2.997420204183892434, 6.110946949555683183 ) ) ;
#7721 = LINE ( 'NONE', #1898, #8815 ) ;
#7722 = CARTESIAN_POINT ( 'NONE',  ( 36.36258059203031934, -19.71368208888610951, 72.86986841596736042 ) ) ;
#7723 = ORIENTED_EDGE ( 'NONE', *, *, #13968, .T. ) ;
#7724 = DIRECTION ( 'NONE',  ( 1.000000000000000000, 0.000000000000000000, 0.000000000000000000 ) ) ;
#7725 = VECTOR ( 'NONE', #2575, 1000.000000000000000 ) ;
#7726 = AXIS2_PLACEMENT_3D ( 'NONE', #8866, #1240, #9122 ) ;
#7727 = DIRECTION ( 'NONE',  ( 1.000000000000000000, 1.734723475976804876E-16, -1.734723475976814737E-16 ) ) ;
#7728 = DIRECTION ( 'NONE',  ( 1.734723475976804876E-16, 3.491481338843135327E-15, 1.000000000000000000 ) ) ;
#7729 = DIRECTION ( 'NONE',  ( 0.000000000000000000, -1.000000000000000000, 3.469446951953617344E-15 ) ) ;
#7730 = LINE ( 'NONE', #17139, #13537 ) ;
#7731 = CARTESIAN_POINT ( 'NONE',  ( 44.81606138205700063, -38.55876147765410167, 72.21586839016146087 ) ) ;
#7732 = CARTESIAN_POINT ( 'NONE',  ( 39.41296390513587511, -13.20384086642191157, 71.08074471024441721 ) ) ;
#7733 = CARTESIAN_POINT ( 'NONE',  ( 37.80618814713140097, 0.08631791111389161553, 73.13360434286904876 ) ) ;
#7734 = ORIENTED_EDGE ( 'NONE', *, *, #711, .F. ) ;
#7735 = CARTESIAN_POINT ( 'NONE',  ( 38.96215273200666473, -22.12380604028318842, 75.81039190382944071 ) ) ;
#7736 = FACE_OUTER_BOUND ( 'NONE', #7405, .T. ) ;
#7737 = ORIENTED_EDGE ( 'NONE', *, *, #20228, .F. ) ;
#7738 = CIRCLE ( 'NONE', #15546, 10.00000000000000000 ) ;
#7739 = ORIENTED_EDGE ( 'NONE', *, *, #24012, .T. ) ;
#7740 = EDGE_CURVE ( 'NONE', #22901, #18207, #4081, .T. ) ;
#7741 = CARTESIAN_POINT ( 'NONE',  ( 39.64521430340305841, -28.80384086642192187, 73.30173637941817333 ) ) ;
#7742 = B_SPLINE_CURVE_WITH_KNOTS ( 'NONE', 3,
 ( #644, #18192, #16626, #20372 ),
 .UNSPECIFIED., .F., .F.,
 ( 4, 4 ),
 ( 0.000000000000000000, 1.000000000000000000 ),
 .UNSPECIFIED. ) ;
#7743 = EDGE_CURVE ( 'NONE', #2757, #13616, #6266, .T. ) ;
#7744 = VECTOR ( 'NONE', #22043, 1000.000000000000000 ) ;
#7745 = PRODUCT_RELATED_PRODUCT_CATEGORY ( 'part', '', ( #7662 ) ) ;
#7746 = CARTESIAN_POINT ( 'NONE',  ( 38.00113996487114321, -25.91368208888609814, 72.53360434286901182 ) ) ;
#7747 = CARTESIAN_POINT ( 'NONE',  ( 36.98690846071097837, -1.813682088886107602, 73.30173637941818754 ) ) ;
#7748 = ORIENTED_EDGE ( 'NONE', *, *, #7774, .F. ) ;
#7749 = DIRECTION ( 'NONE',  ( -1.000000000000000000, 0.000000000000000000, 0.000000000000000000 ) ) ;
#7750 = CARTESIAN_POINT ( 'NONE',  ( 38.93987200065210175, -4.803840866421909439, 72.33091598616827866 ) ) ;
#7751 = CYLINDRICAL_SURFACE ( 'NONE', #15524, 3.000000000000002665 ) ;
#7752 = EDGE_LOOP ( 'NONE', ( #7527, #17071, #12835, #19893 ) ) ;
#7753 = CARTESIAN_POINT ( 'NONE',  ( 40.31606138205700773, -29.30876147765400219, 74.30501292737010033 ) ) ;
#7754 = FACE_OUTER_BOUND ( 'NONE', #13827, .T. ) ;
#7755 = CARTESIAN_POINT ( 'NONE',  ( 36.07789103942399578, -12.20384086642191512, 72.05058123536544201 ) ) ;
#7756 = CARTESIAN_POINT ( 'NONE',  ( 46.81606138205701484, -19.58709462196287632, 24.03834292329984379 ) ) ;
#7757 = CARTESIAN_POINT ( 'NONE',  ( 36.31606138205700773, -21.90577604921434229, 28.73660501626934760 ) ) ;
#7758 = CARTESIAN_POINT ( 'NONE',  ( 39.29254315202756231, -14.81368208888610205, 69.94417936956672577 ) ) ;
#7759 = CARTESIAN_POINT ( 'NONE',  ( 35.31606138205700773, 3.296535697557906985, 65.33616386252352015 ) ) ;
#7760 = CARTESIAN_POINT ( 'NONE',  ( 45.81606138205700063, -34.55876147765410167, 70.30501292737000085 ) ) ;
#7761 = VECTOR ( 'NONE', #8726, 1000.000000000000000 ) ;
#7762 = CYLINDRICAL_SURFACE ( 'NONE', #19628, 0.7500000000000027756 ) ;
#7763 = CARTESIAN_POINT ( 'NONE',  ( 38.26194895904384907, -2.603840866421916367, 73.11602215082118050 ) ) ;
#7764 = PRODUCT_CONTEXT ( 'NONE', #3876, 'mechanical' ) ;
#7765 = CARTESIAN_POINT ( 'NONE',  ( 32.84837986530673248, 3.753595868030215499, 6.230380467512803833 ) ) ;
#7766 = AXIS2_PLACEMENT_3D ( 'NONE', #19307, #15569, #100 ) ;
#7767 = AXIS2_PLACEMENT_3D ( 'NONE', #9168, #10959, #22549 ) ;
#7768 = CARTESIAN_POINT ( 'NONE',  ( 38.93415946300897446, -18.11368208888611164, 73.09843995877329803 ) ) ;
#7769 = LINE ( 'NONE', #10209, #14379 ) ;
#7770 = ADVANCED_FACE ( 'NONE', ( #22444 ), #10260, .F. ) ;
#7771 = VECTOR ( 'NONE', #23229, 1000.000000000000000 ) ;
#7772 = CARTESIAN_POINT ( 'NONE',  ( 40.14115730948191185, -15.10384086642190837, 71.43714994484030001 ) ) ;
#7773 = CARTESIAN_POINT ( 'NONE',  ( 37.31005363372398165, -5.470694883964326571, 83.30188305377672009 ) ) ;
#7774 = EDGE_CURVE ( 'NONE', #17636, #15007, #10383, .T. ) ;
#7775 = CARTESIAN_POINT ( 'NONE',  ( 39.82603832034400426, -20.31368208888610738, 72.40698646996133903 ) ) ;
#7776 = ORIENTED_EDGE ( 'NONE', *, *, #10837, .T. ) ;
#7777 = CARTESIAN_POINT ( 'NONE',  ( 37.61123632939165873, -23.91368208888611235, 73.73360434286898624 ) ) ;
#7778 = ORIENTED_EDGE ( 'NONE', *, *, #15862, .F. ) ;
#7779 = CARTESIAN_POINT ( 'NONE',  ( 38.31606138205700063, -11.98739464995938775, 18.25051608701495809 ) ) ;
#7780 = DIRECTION ( 'NONE',  ( 0.000000000000000000, 2.999999999999999839E-15, 1.000000000000000000 ) ) ;
#7781 = MECHANICAL_DESIGN_GEOMETRIC_PRESENTATION_REPRESENTATION (  '', ( #15978 ), #4086 ) ;
#7782 = CARTESIAN_POINT ( 'NONE',  ( 37.89291511884479036, -24.50384086642190695, 72.49843995877328950 ) ) ;
#7783 = VERTEX_POINT ( 'NONE', #13870 ) ;
#7784 = ORIENTED_EDGE ( 'NONE', *, *, #2685, .T. ) ;
#7785 = DIRECTION ( 'NONE',  ( 1.000000000000000000, 2.999999999999999839E-15, 0.000000000000000000 ) ) ;
#7786 = CYLINDRICAL_SURFACE ( 'NONE', #24792, 0.9999999999999937828 ) ;
#7787 = CARTESIAN_POINT ( 'NONE',  ( 37.61123632939164452, -27.70384086642191690, 69.02690120949091579 ) ) ;
#7788 = AXIS2_PLACEMENT_3D ( 'NONE', #24063, #10427, #15705 ) ;
#7789 = CARTESIAN_POINT ( 'NONE',  ( 38.31606138205700063, 40.69123852234599781, 71.30501292737000085 ) ) ;
#7790 = CARTESIAN_POINT ( 'NONE',  ( 38.37017380507020192, -0.01368208888610778114, 73.71602215082116061 ) ) ;
#7791 = DIRECTION ( 'NONE',  ( -1.000000000000000000, -1.734723475976804876E-16, 1.734723475976814737E-16 ) ) ;
#7792 = ORIENTED_EDGE ( 'NONE', *, *, #15127, .T. ) ;
#7793 = AXIS2_PLACEMENT_3D ( 'NONE', #21764, #21893, #12505 ) ;
#7794 = ORIENTED_EDGE ( 'NONE', *, *, #16305, .F. ) ;
#7795 = CYLINDRICAL_SURFACE ( 'NONE', #10029, 3.999999999999899636 ) ;
#7796 = LINE ( 'NONE', #15643, #3170 ) ;
#7797 = CARTESIAN_POINT ( 'NONE',  ( 37.25202387243754032, -18.40384086642191974, 72.75271321436731853 ) ) ;
#7798 = SURFACE_STYLE_USAGE ( .BOTH. , #9484 ) ;
#7799 = LINE ( 'NONE', #11299, #19449 ) ;
#7800 = VECTOR ( 'NONE', #14954, 1000.000000000000000 ) ;
#7801 = ORIENTED_EDGE ( 'NONE', *, *, #17489, .F. ) ;
#7802 = PLANE ( 'NONE',  #15178 ) ;
#7803 = LINE ( 'NONE', #7675, #21797 ) ;
#7804 = FACE_OUTER_BOUND ( 'NONE', #11944, .T. ) ;
#7805 = CARTESIAN_POINT ( 'NONE',  ( 37.12184278917507640, -8.103840866421910150, 71.32335560751961623 ) ) ;
#7806 = AXIS2_PLACEMENT_3D ( 'NONE', #1389, #16986, #17236 ) ;
#7807 = ORIENTED_EDGE ( 'NONE', *, *, #18261, .F. ) ;
#7808 = CARTESIAN_POINT ( 'NONE',  ( 32.81606138205700773, -27.60498114914039647, 57.04949906928989378 ) ) ;
#7809 = ORIENTED_EDGE ( 'NONE', *, *, #9920, .F. ) ;
#7810 = ORIENTED_EDGE ( 'NONE', *, *, #21240, .F. ) ;
#7811 = CARTESIAN_POINT ( 'NONE',  ( 36.31606138205700063, -29.30876147765401640, 69.30501292737010033 ) ) ;
#7812 = AXIS2_PLACEMENT_3D ( 'NONE', #4729, #22371, #12843 ) ;
#7813 = CARTESIAN_POINT ( 'NONE',  ( 37.25260217561390874, -11.61368208888610098, 71.78268878715392987 ) ) ;
#7814 = CARTESIAN_POINT ( 'NONE',  ( 39.02742774030102879, -14.21368208888610241, 72.26730301774234988 ) ) ;
#7815 = ORIENTED_EDGE ( 'NONE', *, *, #16885, .T. ) ;
#7816 = ORIENTED_EDGE ( 'NONE', *, *, #23410, .F. ) ;
#7817 = DIRECTION ( 'NONE',  ( -1.734723475976804876E-16, -3.491481338843135327E-15, -1.000000000000000000 ) ) ;
#7818 = DIRECTION ( 'NONE',  ( 0.000000000000000000, 1.000000000000000000, 0.000000000000000000 ) ) ;
#7819 = VERTEX_POINT ( 'NONE', #10137 ) ;
#7820 = CARTESIAN_POINT ( 'NONE',  ( 37.31606138205700063, 12.69123852234700678, 71.30501292736997243 ) ) ;
#7821 = CARTESIAN_POINT ( 'NONE',  ( 37.33957961208645315, -15.80384086642190589, 69.94417936956672577 ) ) ;
#7822 = CIRCLE ( 'NONE', #22204, 1.249999999999998890 ) ;
#7823 = CARTESIAN_POINT ( 'NONE',  ( 42.65336712727322777, 3.163553052512885877, 6.379934517999310550 ) ) ;
#7824 = FACE_OUTER_BOUND ( 'NONE', #13421, .T. ) ;
#7825 = CARTESIAN_POINT ( 'NONE',  ( 38.63098279924288647, -18.91368208888609814, 70.22690120949090442 ) ) ;
#7826 = VECTOR ( 'NONE', #8989, 1000.000000000000000 ) ;
#7827 = ORIENTED_EDGE ( 'NONE', *, *, #13984, .T. ) ;
#7828 = DIRECTION ( 'NONE',  ( -1.000000000000000000, 0.000000000000000000, 0.000000000000000000 ) ) ;
#7829 = CARTESIAN_POINT ( 'NONE',  ( 40.14115730948191185, -12.51368208888610489, 71.32335560751960202 ) ) ;
#7830 = CARTESIAN_POINT ( 'NONE',  ( 43.31606138205700063, 2.476587234117772596, 12.62587505415466538 ) ) ;
#7831 = FACE_OUTER_BOUND ( 'NONE', #12456, .T. ) ;
#7832 = VECTOR ( 'NONE', #237, 1000.000000000000000 ) ;
#7833 =( BOUNDED_CURVE ( )  B_SPLINE_CURVE ( 3, ( #13430, #15352, #11376, #13182 ),
 .UNSPECIFIED., .F., .T. ) 
 B_SPLINE_CURVE_WITH_KNOTS ( ( 4, 4 ),
 ( 1.570796326794895004, 3.141592653589793116 ),
 .UNSPECIFIED. ) 
 CURVE ( )  GEOMETRIC_REPRESENTATION_ITEM ( )  RATIONAL_B_SPLINE_CURVE ( ( 1.000000000000000000, 0.8047378541243646044, 0.8047378541243646044, 1.000000000000000000 ) ) 
 REPRESENTATION_ITEM ( '' )  );
#7834 = FACE_BOUND ( 'NONE', #23150, .T. ) ;
#7835 = FACE_OUTER_BOUND ( 'NONE', #21199, .T. ) ;
#7836 = DIRECTION ( 'NONE',  ( 0.000000000000000000, 1.000000000000000000, -3.304235192336775512E-15 ) ) ;
#7837 = ADVANCED_FACE ( 'NONE', ( #10737 ), #21646, .F. ) ;
#7838 =( REPRESENTATION_RELATIONSHIP ('NONE','NONE', #17377, #14735 ) REPRESENTATION_RELATIONSHIP_WITH_TRANSFORMATION ( #1942 )SHAPE_REPRESENTATION_RELATIONSHIP( ) );
#7839 = ORIENTED_EDGE ( 'NONE', *, *, #22859, .T. ) ;
#7840 = ADVANCED_FACE ( 'NONE', ( #1049 ), #1308, .F. ) ;
#7841 = LINE ( 'NONE', #15304, #5782 ) ;
#7842 = ORIENTED_EDGE ( 'NONE', *, *, #18269, .F. ) ;
#7843 = EDGE_CURVE ( 'NONE', #5208, #4227, #9194, .T. ) ;
#7844 = EDGE_LOOP ( 'NONE', ( #19291, #398, #23880, #13400 ) ) ;
#7845 = CARTESIAN_POINT ( 'NONE',  ( 39.73277004305197124, -13.40384086642191619, 69.52238214136768590 ) ) ;
#7846 = EDGE_CURVE ( 'NONE', #9967, #5642, #4928, .T. ) ;
#7847 = ADVANCED_FACE ( 'NONE', ( #24606 ), #6989, .T. ) ;
#7848 = VECTOR ( 'NONE', #20771, 1000.000000000000227 ) ;
#7849 = ORIENTED_EDGE ( 'NONE', *, *, #3407, .F. ) ;
#7850 = DIRECTION ( 'NONE',  ( -4.789116818843729608E-32, 1.000000000000000000, -3.130104260698260371E-15 ) ) ;
#7851 = CARTESIAN_POINT ( 'NONE',  ( 38.26194895904383486, -17.01368208888610312, 69.64448340153877837 ) ) ;
#7852 = VECTOR ( 'NONE', #12097, 1000.000000000000000 ) ;
#7853 = ORIENTED_EDGE ( 'NONE', *, *, #13826, .F. ) ;
#7854 = DIRECTION ( 'NONE',  ( 1.123589211228918605E-15, -0.4425581086832399147, 0.8967398287344627850 ) ) ;
#7855 = PLANE ( 'NONE',  #2204 ) ;
#7856 = EDGE_CURVE ( 'NONE', #23981, #5671, #22296, .T. ) ;
#7857 = CARTESIAN_POINT ( 'NONE',  ( 36.89935272106204422, -13.21368208888610241, 69.52238214136768590 ) ) ;
#7858 = EDGE_CURVE ( 'NONE', #19743, #6874, #11501, .T. ) ;
#7859 = ORIENTED_EDGE ( 'NONE', *, *, #23995, .T. ) ;
#7860 = FILL_AREA_STYLE_COLOUR ( '', #1192 ) ;
#7861 = DIRECTION ( 'NONE',  ( 1.000000000000000275E-15, -0.9439899321577401858, -0.3299742535180970604 ) ) ;
#7862 = PLANE ( 'NONE',  #22373 ) ;
#7863 = AXIS2_PLACEMENT_3D ( 'NONE', #14184, #6064, #12135 ) ;
#7864 = CARTESIAN_POINT ( 'NONE',  ( 36.31606138205699352, 5.691238522346986350, 65.51211970855653988 ) ) ;
#7865 = DIRECTION ( 'NONE',  ( 1.000000000000000000, 0.000000000000000000, -0.000000000000000000 ) ) ;
#7866 = VECTOR ( 'NONE', #17219, 1000.000000000000000 ) ;
#7867 = CARTESIAN_POINT ( 'NONE',  ( 39.41296390513587511, -11.20384086642191335, 71.08074471024443142 ) ) ;
#7868 = CARTESIAN_POINT ( 'NONE',  ( 39.82603832034400426, 1.686317911113891732, 72.40698646996136745 ) ) ;
#7869 = ORIENTED_EDGE ( 'NONE', *, *, #1081, .F. ) ;
#7870 = FACE_OUTER_BOUND ( 'NONE', #8511, .T. ) ;
#7871 = CARTESIAN_POINT ( 'NONE',  ( 44.81606138205700063, 35.44123852234597649, 68.30501292736990138 ) ) ;
#7872 = ORIENTED_EDGE ( 'NONE', *, *, #5809, .F. ) ;
#7873 = ORIENTED_EDGE ( 'NONE', *, *, #5424, .F. ) ;
#7874 = CARTESIAN_POINT ( 'NONE',  ( 37.33957961208645315, -1.803840866421907441, 69.94417936956673998 ) ) ;
#7875 = CARTESIAN_POINT ( 'NONE',  ( 37.38336156205274818, -23.71368208888610241, 72.12822762946747446 ) ) ;
#7876 = PRODUCT ( 'MAS-155', 'MAS-155', '', ( #14848 ) ) ;
#7877 = CARTESIAN_POINT ( 'NONE',  ( 37.50301148336529167, -3.113682088886100097, 69.06206559358666652 ) ) ;
#7878 = VERTEX_POINT ( 'NONE', #5566 ) ;
#7879 = DIRECTION ( 'NONE',  ( -1.000000000000000078E-15, 0.9439899321577400748, 0.3299742535180970049 ) ) ;
#7880 = CARTESIAN_POINT ( 'NONE',  ( 39.98359781491296161, -27.20384086642191335, 70.89533451361944572 ) ) ;
#7881 = CARTESIAN_POINT ( 'NONE',  ( 45.81606138205700063, -26.74044063519535186, 84.30501292737007191 ) ) ;
#7882 = EDGE_LOOP ( 'NONE', ( #7792, #5807, #2471, #13753 ) ) ;
#7883 = DIRECTION ( 'NONE',  ( -7.570943305532639295E-31, -1.000000000000000000, -4.914813388431354887E-16 ) ) ;
#7884 = DIRECTION ( 'NONE',  ( 0.000000000000000000, 1.000000000000000000, 0.000000000000000000 ) ) ;
#7885 = CARTESIAN_POINT ( 'NONE',  ( 36.29569395875881099, -10.30384086642191832, 72.77780686321129622 ) ) ;
#7886 = DIRECTION ( 'NONE',  ( 0.000000000000000000, -1.000000000000000000, 4.625929269271485322E-15 ) ) ;
#7887 = CARTESIAN_POINT ( 'NONE',  ( 32.56606138205700773, 40.39281886181299797, 84.30501292736984453 ) ) ;
#7888 = CARTESIAN_POINT ( 'NONE',  ( 39.95015449827720744, -16.61368208888610454, 70.79240656858105751 ) ) ;
#7889 = PLANE ( 'NONE',  #7298 ) ;
#7890 = CIRCLE ( 'NONE', #472, 2.500000000000002220 ) ;
#7891 = CARTESIAN_POINT ( 'NONE',  ( 37.69796330110504101, -25.11368208888609743, 69.66206559358661821 ) ) ;
#7892 = DIRECTION ( 'NONE',  ( 0.000000000000000000, -0.7540134720837687876, -0.6568589528324780824 ) ) ;
#7893 = EDGE_CURVE ( 'NONE', #11682, #17758, #20653, .T. ) ;
#7894 = CARTESIAN_POINT ( 'NONE',  ( 36.80608444377002542, -0.3038408664219130473, 72.40698646996135324 ) ) ;
#7895 = EDGE_CURVE ( 'NONE', #1085, #11430, #15473, .T. ) ;
#7896 = ITEM_DEFINED_TRANSFORMATION ( 'NONE', 'NONE', #1822,  #2000 ) ;
#7897 = FACE_OUTER_BOUND ( 'NONE', #16176, .T. ) ;
#7898 = CARTESIAN_POINT ( 'NONE',  ( 38.93415946300897446, -20.11368208888610809, 73.09843995877329803 ) ) ;
#7899 = PLANE ( 'NONE',  #16844 ) ;
#7900 = CARTESIAN_POINT ( 'NONE',  ( 37.25202387243754032, -20.40384086642191619, 72.75271321436731853 ) ) ;
#7901 = PLANE ( 'NONE',  #11409 ) ;
#7902 = CIRCLE ( 'NONE', #22270, 0.4999999999999982792 ) ;
#7903 = CARTESIAN_POINT ( 'NONE',  ( 39.82603832034400426, -10.31368208888610383, 72.40698646996135324 ) ) ;
#7904 = VERTEX_POINT ( 'NONE', #21657 ) ;
#7905 = CARTESIAN_POINT ( 'NONE',  ( 39.64521430340304420, -24.81368208888610738, 69.45876917294174291 ) ) ;
#7906 = EDGE_LOOP ( 'NONE', ( #19429, #11144, #23693, #6823 ) ) ;
#7907 = LINE ( 'NONE', #23474, #23835 ) ;
#7908 = LINE ( 'NONE', #19364, #16997 ) ;
#7909 = CARTESIAN_POINT ( 'NONE',  ( 38.93987200065210175, -24.80384086642191477, 72.33091598616823603 ) ) ;
#7910 = ORIENTED_EDGE ( 'NONE', *, *, #16177, .T. ) ;
#7911 = ORIENTED_EDGE ( 'NONE', *, *, #15703, .T. ) ;
#7912 = DIRECTION ( 'NONE',  ( 0.000000000000000000, -0.4425581086832391930, 0.8967398287344632291 ) ) ;
#7913 = DIRECTION ( 'NONE',  ( 0.000000000000000000, -1.000000000000000000, 2.999999999999999839E-15 ) ) ;
#7914 = CARTESIAN_POINT ( 'NONE',  ( 36.49096545463212493, -0.1038408664219107880, 71.32335560751963044 ) ) ;
#7915 = SURFACE_SIDE_STYLE ('',( #8844 ) ) ;
#7916 = CARTESIAN_POINT ( 'NONE',  ( 40.26954217208371034, -2.713682088886101962, 69.89063713639259845 ) ) ;
#7917 = VECTOR ( 'NONE', #10864, 1000.000000000000000 ) ;
#7918 = PLANE ( 'NONE',  #20475 ) ;
#7919 = AXIS2_PLACEMENT_3D ( 'NONE', #9006, #16853, #24435 ) ;
#7920 = ORIENTED_EDGE ( 'NONE', *, *, #13378, .F. ) ;
#7921 = EDGE_CURVE ( 'NONE', #24841, #22626, #13425, .T. ) ;
#7922 = ORIENTED_EDGE ( 'NONE', *, *, #711, .T. ) ;
#7923 = ADVANCED_FACE ( 'NONE', ( #7496 ), #23321, .F. ) ;
#7924 = CARTESIAN_POINT ( 'NONE',  ( 33.63983381732882805, 3.338985100189890254, 6.348312178689752727 ) ) ;
#7925 = CARTESIAN_POINT ( 'NONE',  ( 43.81606138205700063, 41.44123852234598360, 71.05501292736988717 ) ) ;
#7926 = EDGE_CURVE ( 'NONE', #19611, #17400, #4119, .T. ) ;
#7927 = CIRCLE ( 'NONE', #7494, 1.800000000000002931 ) ;
#7928 = CARTESIAN_POINT ( 'NONE',  ( 38.26194895904384907, -22.60384086642191548, 73.11602215082116629 ) ) ;
#7929 = PRESENTATION_STYLE_ASSIGNMENT (( #13844 ) ) ;
#7930 = CARTESIAN_POINT ( 'NONE',  ( 38.31606138205712853, 42.19123852234595518, 61.30501292736988006 ) ) ;
#7931 = VERTEX_POINT ( 'NONE', #10076 ) ;
#7932 = DIRECTION ( 'NONE',  ( -1.000000000000000000, -3.091505625455828697E-15, -4.515976121274772923E-17 ) ) ;
#7933 = VECTOR ( 'NONE', #5411, 1000.000000000000000 ) ;
#7934 = CARTESIAN_POINT ( 'NONE',  ( 32.81606138205700773, -27.66931681479738003, 59.51410614687260647 ) ) ;
#7935 = ORIENTED_EDGE ( 'NONE', *, *, #5779, .T. ) ;
#7936 = CARTESIAN_POINT ( 'NONE',  ( 39.24876120206129571, -6.903840866421912636, 72.12822762946750288 ) ) ;
#7937 = DIRECTION ( 'NONE',  ( -0.000000000000000000, -3.469446951953613400E-15, -1.000000000000000000 ) ) ;
#7938 = VERTEX_POINT ( 'NONE', #25248 ) ;
#7939 = EDGE_CURVE ( 'NONE', #7305, #16039, #24667, .T. ) ;
#7940 = DIRECTION ( 'NONE',  ( 1.000000000000000000, 2.999999999999999839E-15, 0.000000000000000000 ) ) ;
#7941 = VERTEX_POINT ( 'NONE', #23707 ) ;
#7942 = ORIENTED_EDGE ( 'NONE', *, *, #5648, .F. ) ;
#7943 = AXIS2_PLACEMENT_3D ( 'NONE', #460, #23907, #22237 ) ;
#7944 = DIRECTION ( 'NONE',  ( -0.1733269559585470521, -3.077057697073492856E-15, -0.9848643390529193686 ) ) ;
#7945 = CARTESIAN_POINT ( 'NONE',  ( 37.89291511884476904, -11.11368208888610276, 70.26206559358664094 ) ) ;
#7946 = CARTESIAN_POINT ( 'NONE',  ( 38.93987200065208754, -10.81368208888610027, 70.42958956619168021 ) ) ;
#7947 = ORIENTED_EDGE ( 'NONE', *, *, #5246, .F. ) ;
#7948 = EDGE_LOOP ( 'NONE', ( #17311, #19488, #6108, #21449 ) ) ;
#7949 = CARTESIAN_POINT ( 'NONE',  ( 43.06606138205700063, 41.44123852234599781, 75.30501292736987295 ) ) ;
#7950 = AXIS2_PLACEMENT_3D ( 'NONE', #8453, #23894, #19920 ) ;
#7951 = CARTESIAN_POINT ( 'NONE',  ( 32.81606138205700773, -33.39268706791821728, 60.15578316240965506 ) ) ;
#7952 = EDGE_LOOP ( 'NONE', ( #13257, #15522, #18354, #1606 ) ) ;
#7953 = LINE ( 'NONE', #21724, #21044 ) ;
#7954 = CARTESIAN_POINT ( 'NONE',  ( 38.82593461698265003, -16.70384086642191690, 73.13360434286903455 ) ) ;
#7955 = CARTESIAN_POINT ( 'NONE',  ( 36.31606138205700063, -20.44571330440884793, 75.97665497822788438 ) ) ;
#7956 = VECTOR ( 'NONE', #7961, 1000.000000000000000 ) ;
#7957 = LINE ( 'NONE', #2132, #19099 ) ;
#7958 = CARTESIAN_POINT ( 'NONE',  ( 39.02742774030102879, -16.21368208888609885, 72.26730301774234988 ) ) ;
#7959 = ORIENTED_EDGE ( 'NONE', *, *, #7740, .T. ) ;
#7960 = ORIENTED_EDGE ( 'NONE', *, *, #3252, .F. ) ;
#7961 = DIRECTION ( 'NONE',  ( 3.491481338843135327E-15, 1.000000000000000000, -2.999999999999999839E-15 ) ) ;
#7962 = CARTESIAN_POINT ( 'NONE',  ( 38.82593461698262871, -16.91368208888609814, 69.62690120949091011 ) ) ;
#7963 = AXIS2_PLACEMENT_3D ( 'NONE', #19879, #16374, #17956 ) ;
#7964 = DIRECTION ( 'NONE',  ( -1.000000000000000000, -2.999999999999999839E-15, 0.000000000000000000 ) ) ;
#7965 = AXIS2_PLACEMENT_3D ( 'NONE', #14476, #16524, #12567 ) ;
#7966 = CARTESIAN_POINT ( 'NONE',  ( 44.81606138205700063, -34.55876147765400930, 73.30501292737011454 ) ) ;
#7967 = CARTESIAN_POINT ( 'NONE',  ( 39.38009889167650357, -28.21368208888610951, 72.75271321436730432 ) ) ;
#7968 = CARTESIAN_POINT ( 'NONE',  ( 36.81465384343994884, 40.95934826813394380, 79.52109337493037344 ) ) ;
#7969 = AXIS2_PLACEMENT_3D ( 'NONE', #1704, #13707, #21685 ) ;
#7970 = PLANE ( 'NONE',  #4910 ) ;
#7971 = ORIENTED_EDGE ( 'NONE', *, *, #5256, .T. ) ;
#7972 = CIRCLE ( 'NONE', #1371, 0.5000000000000022204 ) ;
#7973 = EDGE_CURVE ( 'NONE', #9136, #3785, #2454, .T. ) ;
#7974 = DIRECTION ( 'NONE',  ( 2.602085213965210642E-15, -0.8967398287344635621, -0.4425581086832386379 ) ) ;
#7975 = ORIENTED_EDGE ( 'NONE', *, *, #5626, .T. ) ;
#7976 = ORIENTED_EDGE ( 'NONE', *, *, #1979, .F. ) ;
#7977 = CARTESIAN_POINT ( 'NONE',  ( 39.02088643472237806, -6.703840866421919564, 73.73360434286902887 ) ) ;
#7978 = COLOUR_RGB ( '', 0.40784314, 0.44705882, 0.49803922) ;
#7979 = EDGE_LOOP ( 'NONE', ( #10791, #19680, #7159, #2933 ) ) ;
#7980 = FACE_OUTER_BOUND ( 'NONE', #5292, .T. ) ;
#7981 = CARTESIAN_POINT ( 'NONE',  ( 39.98359781491296161, -8.413682088886105248, 71.86517103874048473 ) ) ;
#7982 = AXIS2_PLACEMENT_3D ( 'NONE', #6583, #14686, #10960 ) ;
#7983 = ORIENTED_EDGE ( 'NONE', *, *, #6903, .F. ) ;
#7984 = PLANE ( 'NONE',  #21509 ) ;
#7985 = VECTOR ( 'NONE', #19720, 1000.000000000000000 ) ;
#7986 = CARTESIAN_POINT ( 'NONE',  ( 38.37017380507020192, -16.01368208888610667, 73.71602215082113219 ) ) ;
#7987 = ADVANCED_FACE ( 'NONE', ( #136 ), #11885, .T. ) ;
#7988 = DIRECTION ( 'NONE',  ( 0.000000000000000000, 0.3299742535180963943, -0.9439899321577402969 ) ) ;
#7989 = CARTESIAN_POINT ( 'NONE',  ( 40.31606138205700773, -11.51539968388051705, 18.41550321377400934 ) ) ;
#7990 = AXIS2_PLACEMENT_3D ( 'NONE', #5196, #14981, #17778 ) ;
#7991 = DIRECTION ( 'NONE',  ( 0.000000000000000000, -2.999999999999999839E-15, -1.000000000000000000 ) ) ;
#7992 = ADVANCED_FACE ( 'NONE', ( #9946 ), #3747, .F. ) ;
#7993 = CARTESIAN_POINT ( 'NONE',  ( 34.06606138205700773, -39.60075215179220720, 69.23691647014479145 ) ) ;
#7994 = CIRCLE ( 'NONE', #8416, 2.000000000000001776 ) ;
#7995 = FACE_OUTER_BOUND ( 'NONE', #13172, .T. ) ;
#7996 = CARTESIAN_POINT ( 'NONE',  ( 38.00113996487112189, -13.70384086642191157, 70.22690120949090442 ) ) ;
#7997 = CARTESIAN_POINT ( 'NONE',  ( 39.41296390513587511, -22.41368208888610525, 71.67976084211551324 ) ) ;
#7998 = ORIENTED_EDGE ( 'NONE', *, *, #22449, .F. ) ;
#7999 = LINE ( 'NONE', #13912, #19315 ) ;
#8000 = VECTOR ( 'NONE', #5350, 1000.000000000000114 ) ;
#8001 = EDGE_CURVE ( 'NONE', #19553, #7819, #5952, .T. ) ;
#8002 = CYLINDRICAL_SURFACE ( 'NONE', #23442, 2.000000000000000000 ) ;
#8003 = ORIENTED_EDGE ( 'NONE', *, *, #21070, .F. ) ;
#8004 = ORIENTED_EDGE ( 'NONE', *, *, #2002, .F. ) ;
#8005 = CARTESIAN_POINT ( 'NONE',  ( 37.61123632939164452, -21.70384086642190979, 69.02690120949091579 ) ) ;
#8006 = CARTESIAN_POINT ( 'NONE',  ( 38.63098279924288647, -26.91368208888610170, 70.22690120949089021 ) ) ;
#8007 = CARTESIAN_POINT ( 'NONE',  ( 35.86008812008917346, -3.513682088886104005, 71.43714994484035685 ) ) ;
#8008 = ORIENTED_EDGE ( 'NONE', *, *, #6282, .T. ) ;
#8009 = CARTESIAN_POINT ( 'NONE',  ( 34.66606138205693810, 6.548188142891429919, 4.975198841308384523 ) ) ;
#8010 = CARTESIAN_POINT ( 'NONE',  ( 37.69225076346193504, -1.803840866421911215, 70.42958956619168021 ) ) ;
#8011 = CARTESIAN_POINT ( 'NONE',  ( 46.81606138205695089, 5.290470704224636833, -0.3848988112044732235 ) ) ;
#8012 = ORIENTED_EDGE ( 'NONE', *, *, #24661, .T. ) ;
#8013 = DIRECTION ( 'NONE',  ( 1.000000000000000000, 1.950367120401949903E-17, -2.478176394252580155E-16 ) ) ;
#8014 = CARTESIAN_POINT ( 'NONE',  ( 43.81606138205700063, -34.55876147765707174, 70.30501292736873609 ) ) ;
#8015 = CARTESIAN_POINT ( 'NONE',  ( 40.26954217208372455, -4.903840866421919742, 72.86986841596736042 ) ) ;
#8016 = VECTOR ( 'NONE', #23226, 1000.000000000000227 ) ;
#8017 = DIRECTION ( 'NONE',  ( 0.000000000000000000, 0.5706330172266919076, -0.8212051873014208914 ) ) ;
#8018 = LINE ( 'NONE', #8132, #51 ) ;
#8019 = CARTESIAN_POINT ( 'NONE',  ( 36.68196826583682935, -5.613682088886105426, 71.96809898377890136 ) ) ;
#8020 = CYLINDRICAL_SURFACE ( 'NONE', #14208, 0.7500000000000008882 ) ;
#8021 = EDGE_CURVE ( 'NONE', #23179, #18040, #1677, .T. ) ;
#8022 = CARTESIAN_POINT ( 'NONE',  ( 36.80608444377001121, -27.31368208888610383, 70.35351908239857721 ) ) ;
#8023 = EDGE_CURVE ( 'NONE', #6791, #12100, #25375, .T. ) ;
#8024 = DIRECTION ( 'NONE',  ( -1.000000000000000000, -1.497661361212515810E-15, -3.239770556388344395E-15 ) ) ;
#8025 = CARTESIAN_POINT ( 'NONE',  ( 39.75915168707251723, -2.903840866421914413, 72.49904802271740323 ) ) ;
#8026 = DIRECTION ( 'NONE',  ( 0.9848643390529194797, -5.199808678756412277E-16, -0.1733269559585470798 ) ) ;
#8027 = CARTESIAN_POINT ( 'NONE',  ( 36.64852494920107517, -17.41368208888610525, 70.89533451361947414 ) ) ;
#8028 = CARTESIAN_POINT ( 'NONE',  ( 38.31606138205700063, -4.399276463885007260, 59.51717649063222382 ) ) ;
#8029 = EDGE_CURVE ( 'NONE', #12177, #20637, #7631, .T. ) ;
#8030 = AXIS2_PLACEMENT_3D ( 'NONE', #12922, #18710, #11112 ) ;
#8031 = CARTESIAN_POINT ( 'NONE',  ( 37.80618814713138676, -11.70384086642190624, 69.62690120949091011 ) ) ;
#8032 = CARTESIAN_POINT ( 'NONE',  ( 39.75915168707250302, -10.71368208888609885, 70.26145752964252722 ) ) ;
#8033 = EDGE_LOOP ( 'NONE', ( #15489, #24827, #2025, #12207 ) ) ;
#8034 = CARTESIAN_POINT ( 'NONE',  ( 40.77203464402485622, -22.51368208888610667, 71.32335560751960202 ) ) ;
#8035 = ORIENTED_EDGE ( 'NONE', *, *, #889, .F. ) ;
#8036 = LINE ( 'NONE', #17695, #10699 ) ;
#8037 = CYLINDRICAL_SURFACE ( 'NONE', #4653, 0.9999999999999937828 ) ;
#8038 = CARTESIAN_POINT ( 'NONE',  ( 39.02742774030101458, -15.40384086642191441, 70.49320253461759478 ) ) ;
#8039 = ORIENTED_EDGE ( 'NONE', *, *, #10589, .F. ) ;
#8040 = EDGE_CURVE ( 'NONE', #20004, #1510, #3884, .T. ) ;
#8041 = ORIENTED_EDGE ( 'NONE', *, *, #11635, .T. ) ;
#8042 = DIRECTION ( 'NONE',  ( -1.000000000000000000, 0.000000000000000000, 0.000000000000000000 ) ) ;
#8043 = CARTESIAN_POINT ( 'NONE',  ( 33.31606138205700773, -29.06829118875199924, 75.80501292737000085 ) ) ;
#8044 = CARTESIAN_POINT ( 'NONE',  ( 39.02088643472237806, -20.70384086642192401, 73.73360434286898624 ) ) ;
#8045 = DIRECTION ( 'NONE',  ( 7.071067811865460542E-16, -0.4341746501209495790, -0.9008287146801832179 ) ) ;
#8046 = CARTESIAN_POINT ( 'NONE',  ( 40.33642880535524000, -4.313682088886108268, 72.77780686321128201 ) ) ;
#8047 = CARTESIAN_POINT ( 'NONE',  ( 44.06606138205700063, 40.39281886181299797, 82.55501292736983032 ) ) ;
#8048 = AXIS2_PLACEMENT_3D ( 'NONE', #133, #8013, #5683 ) ;
#8049 = ORIENTED_EDGE ( 'NONE', *, *, #17211, .T. ) ;
#8050 = CARTESIAN_POINT ( 'NONE',  ( 35.81606138205700063, -24.05876147765400219, 74.30501292737008612 ) ) ;
#8051 = LINE ( 'NONE', #14347, #269 ) ;
#8052 = CARTESIAN_POINT ( 'NONE',  ( 38.93415946300897446, -19.50384086642190695, 69.66206559358663242 ) ) ;
#8053 =( NAMED_UNIT ( * ) SI_UNIT ( $, .STERADIAN. ) SOLID_ANGLE_UNIT ( ) );
#8054 = CARTESIAN_POINT ( 'NONE',  ( 44.81606138205700063, -34.55876147765400930, 73.30501292737011454 ) ) ;
#8055 = ORIENTED_EDGE ( 'NONE', *, *, #19946, .F. ) ;
#8056 = FACE_OUTER_BOUND ( 'NONE', #5739, .T. ) ;
#8057 = LINE ( 'NONE', #6378, #16036 ) ;
#8058 = EDGE_LOOP ( 'NONE', ( #22523, #13290, #11880, #4484 ) ) ;
#8059 = CARTESIAN_POINT ( 'NONE',  ( 38.26194895904384197, -6.603840866421913702, 72.51602215082118619 ) ) ;
#8060 = DIRECTION ( 'NONE',  ( 1.000000000000000078E-15, -0.9439899321577417401, -0.3299742535180921199 ) ) ;
#8061 = VERTEX_POINT ( 'NONE', #4146 ) ;
#8062 = CARTESIAN_POINT ( 'NONE',  ( 33.31606138205700773, -27.25871422114667553, 59.79942265548595515 ) ) ;
#8063 = VERTEX_POINT ( 'NONE', #25114 ) ;
#8064 = ORIENTED_EDGE ( 'NONE', *, *, #1119, .T. ) ;
#8066 = ADVANCED_FACE ( 'NONE', ( #9698, #14191 ), #24081, .F. ) ;
#8065 = FACE_OUTER_BOUND ( 'NONE', #23914, .T. ) ;
#8067 = CARTESIAN_POINT ( 'NONE',  ( 37.89291511884476904, -3.113682088886100097, 70.26206559358664094 ) ) ;
#8068 = EDGE_CURVE ( 'NONE', #17340, #10765, #2314, .T. ) ;
#8069 = CARTESIAN_POINT ( 'NONE',  ( 38.26194895904383486, -3.013682088886100008, 70.24448340153877268 ) ) ;
#8070 = ORIENTED_EDGE ( 'NONE', *, *, #13175, .T. ) ;
#8071 = EDGE_CURVE ( 'NONE', #18383, #4779, #22284, .T. ) ;
#8072 = ORIENTED_EDGE ( 'NONE', *, *, #12737, .F. ) ;
#8073 = LINE ( 'NONE', #6135, #1264 ) ;
#8074 = FACE_OUTER_BOUND ( 'NONE', #12506, .T. ) ;
#8075 = ORIENTED_EDGE ( 'NONE', *, *, #4143, .T. ) ;
#8076 = DIRECTION ( 'NONE',  ( 1.734723475976804876E-16, 3.269436733918100469E-15, 1.000000000000000000 ) ) ;
#8077 = CARTESIAN_POINT ( 'NONE',  ( 39.38009889167648936, -15.40384086642190908, 70.00779233799262613 ) ) ;
#8078 = LINE ( 'NONE', #12076, #22705 ) ;
#8079 = CARTESIAN_POINT ( 'NONE',  ( 38.31606138205700063, -29.78523130861184143, 52.92072663988442116 ) ) ;
#8080 = FACE_OUTER_BOUND ( 'NONE', #19384, .T. ) ;
#8081 = ORIENTED_EDGE ( 'NONE', *, *, #9594, .T. ) ;
#8082 = ORIENTED_EDGE ( 'NONE', *, *, #21225, .T. ) ;
#8083 = DIRECTION ( 'NONE',  ( 0.000000000000000000, 1.000000000000000000, -2.999999999999998655E-15 ) ) ;
#8084 = CARTESIAN_POINT ( 'NONE',  ( 39.98359781491296161, -16.41368208888610525, 71.86517103874047052 ) ) ;
#8085 = EDGE_CURVE ( 'NONE', #21126, #17867, #8649, .T. ) ;
#8086 = DIRECTION ( 'NONE',  ( -1.000000000000000000, 0.000000000000000000, 0.000000000000000000 ) ) ;
#8087 = CARTESIAN_POINT ( 'NONE',  ( 40.31606138205700773, -1.357181138186128067, 82.80501292736991559 ) ) ;
#8088 = DIRECTION ( 'NONE',  ( -2.048868001712899108E-15, 0.6595716529892353686, -0.7516416929448815898 ) ) ;
#8089 = CARTESIAN_POINT ( 'NONE',  ( 40.31606138205698642, -8.139132291388515128, 32.47600601670134779 ) ) ;
#8090 = PRODUCT_DEFINITION_SHAPE ( 'NONE', 'NONE',  #11212 ) ;
#8091 = DIRECTION ( 'NONE',  ( -1.000000000000000000, -2.556434596176347380E-15, -1.460819769243627131E-15 ) ) ;
#8092 = CARTESIAN_POINT ( 'NONE',  ( 36.31606138205700063, -29.06829118875199924, 75.80501292737000085 ) ) ;
#8093 = EDGE_LOOP ( 'NONE', ( #15997, #16811, #6632, #24378 ) ) ;
#8094 = DIRECTION ( 'NONE',  ( 0.000000000000000000, 1.000000000000000000, 0.000000000000000000 ) ) ;
#8095 = ORIENTED_EDGE ( 'NONE', *, *, #12104, .F. ) ;
#8096 = ORIENTED_EDGE ( 'NONE', *, *, #22081, .F. ) ;
#8097 = CARTESIAN_POINT ( 'NONE',  ( 37.61123632939164452, -5.703840866421911571, 69.02690120949094421 ) ) ;
#8098 = EDGE_LOOP ( 'NONE', ( #10774, #22472, #6191, #15716 ) ) ;
#8099 = FACE_OUTER_BOUND ( 'NONE', #24777, .T. ) ;
#8100 = CARTESIAN_POINT ( 'NONE',  ( 36.64852494920107517, -7.413682088886104360, 70.89533451361948835 ) ) ;
#8101 = VERTEX_POINT ( 'NONE', #4766 ) ;
#8102 = CARTESIAN_POINT ( 'NONE',  ( 42.56606138205700063, -32.75315594507191008, 59.38245422252773409 ) ) ;
#8103 = CARTESIAN_POINT ( 'NONE',  ( 39.73277004305198545, -14.21368208888610951, 73.23812341099225875 ) ) ;
#8104 = DIRECTION ( 'NONE',  ( 1.000000000000000000, -1.301042606982604682E-30, -4.336808689942015271E-16 ) ) ;
#8105 = CARTESIAN_POINT ( 'NONE',  ( 32.81606138205700773, 4.124002793203064066, 6.312068993173404863 ) ) ;
#8106 = EDGE_CURVE ( 'NONE', #19369, #23504, #10194, .T. ) ;
#8107 = AXIS2_PLACEMENT_3D ( 'NONE', #826, #2884, #18749 ) ;
#8108 = CARTESIAN_POINT ( 'NONE',  ( 43.30251437062377562, 3.928705369154989135, 6.336397002151890057 ) ) ;
#8109 = AXIS2_PLACEMENT_3D ( 'NONE', #12558, #20393, #1054 ) ;
#8110 = AXIS2_PLACEMENT_3D ( 'NONE', #19995, #2333, #4411 ) ;
#8111 = DIRECTION ( 'NONE',  ( -1.000000000000000000, 0.000000000000000000, 0.000000000000000000 ) ) ;
#8112 = DIRECTION ( 'NONE',  ( -2.048868001712896742E-15, 0.6595716529892345914, -0.7516416929448823669 ) ) ;
#8113 = DIRECTION ( 'NONE',  ( 1.000000000000000000, 0.000000000000000000, 0.000000000000000000 ) ) ;
#8114 = CARTESIAN_POINT ( 'NONE',  ( 37.38336156205274818, -23.71368208888610241, 72.12822762946747446 ) ) ;
#8115 = ORIENTED_EDGE ( 'NONE', *, *, #23403, .T. ) ;
#8116 = FACE_OUTER_BOUND ( 'NONE', #8355, .T. ) ;
#8117 = LINE ( 'NONE', #23815, #7011 ) ;
#8118 = ORIENTED_EDGE ( 'NONE', *, *, #6807, .F. ) ;
#8119 = VERTEX_POINT ( 'NONE', #2818 ) ;
#8120 = CARTESIAN_POINT ( 'NONE',  ( 36.36258059203030513, -23.90384086642191619, 69.89063713639258424 ) ) ;
#8121 = CARTESIAN_POINT ( 'NONE',  ( 39.95015449827720744, -26.61368208888610809, 70.79240656858104330 ) ) ;
#8122 = LINE ( 'NONE', #4636, #7027 ) ;
#8123 = PRESENTATION_LAYER_ASSIGNMENT (  '', '', ( #9371 ) ) ;
#8124 = AXIS2_PLACEMENT_3D ( 'NONE', #3122, #19108, #24997 ) ;
#8125 = AXIS2_PLACEMENT_3D ( 'NONE', #4068, #11425, #2118 ) ;
#8126 = DIRECTION ( 'NONE',  ( 0.000000000000000000, 0.5706330172266920187, -0.8212051873014210024 ) ) ;
#8127 = EDGE_LOOP ( 'NONE', ( #8205, #21422, #7313, #12080 ) ) ;
#8128 = CYLINDRICAL_SURFACE ( 'NONE', #2271, 0.4999999999999982792 ) ;
#8129 = CARTESIAN_POINT ( 'NONE',  ( 38.09940268710882094, 38.69123852234599781, 70.07393250355386272 ) ) ;
#8130 = CARTESIAN_POINT ( 'NONE',  ( 38.37017380507018771, -1.603840866421912148, 69.04448340153881247 ) ) ;
#8131 = CARTESIAN_POINT ( 'NONE',  ( 31.81606138205700418, 40.39281886181299797, 82.55501292736983032 ) ) ;
#8132 = CARTESIAN_POINT ( 'NONE',  ( 35.31606138205700773, 3.099306811489555891, 65.29760936252343129 ) ) ;
#8133 = CARTESIAN_POINT ( 'NONE',  ( 40.14115730948191185, -4.513682088886103116, 71.32335560751961623 ) ) ;
#8134 = DIRECTION ( 'NONE',  ( 1.327674326049719602E-15, -0.4425581086832399147, 0.8967398287344627850 ) ) ;
#8135 = LINE ( 'NONE', #4277, #4806 ) ;
#8136 = DIRECTION ( 'NONE',  ( -1.734723475976804876E-16, -3.469446951953620105E-15, -1.000000000000000000 ) ) ;
#8137 = CARTESIAN_POINT ( 'NONE',  ( 38.93415946300897446, -1.503840866421909173, 69.66206559358664663 ) ) ;
#8138 = AXIS2_PLACEMENT_3D ( 'NONE', #24318, #8509, #22409 ) ;
#8139 = ITEM_DEFINED_TRANSFORMATION ( 'NONE', 'NONE', #4313,  #2000 ) ;
#8140 = CARTESIAN_POINT ( 'NONE',  ( 40.64099152588522657, -0.6071811381869983704, 82.55501292736998664 ) ) ;
#8141 = CARTESIAN_POINT ( 'NONE',  ( 37.60469502381300799, -28.40384086642191264, 72.26730301774232146 ) ) ;
#8142 = CARTESIAN_POINT ( 'NONE',  ( 36.80608444377001121, -9.313682088886100274, 70.35351908239860563 ) ) ;
#8143 = AXIS2_PLACEMENT_3D ( 'NONE', #1969, #13342, #5472 ) ;
#8144 = VECTOR ( 'NONE', #20558, 1000.000000000000114 ) ;
#8145 = CARTESIAN_POINT ( 'NONE',  ( 46.81606138205707168, -36.31746077171913356, 73.86860304758450013 ) ) ;
#8146 = CARTESIAN_POINT ( 'NONE',  ( 36.49096545463212493, -10.10384086642191193, 71.32335560751963044 ) ) ;
#8147 = EDGE_CURVE ( 'NONE', #16154, #20256, #6177, .T. ) ;
#8148 = DIRECTION ( 'NONE',  ( 1.000000000000000000, 2.999999999999999839E-15, 0.000000000000000000 ) ) ;
#8149 = ADVANCED_FACE ( 'NONE', ( #4646 ), #20484, .T. ) ;
#8150 = CARTESIAN_POINT ( 'NONE',  ( 36.80608444377001121, -9.313682088886100274, 70.35351908239860563 ) ) ;
#8151 = VERTEX_POINT ( 'NONE', #10451 ) ;
#8152 = CARTESIAN_POINT ( 'NONE',  ( 35.86008812008917346, -17.51368208888610667, 71.43714994484034264 ) ) ;
#8153 = ORIENTED_EDGE ( 'NONE', *, *, #2008, .T. ) ;
#8154 = DIRECTION ( 'NONE',  ( 0.000000000000000000, 0.5706330172266919076, -0.8212051873014208914 ) ) ;
#8155 = EDGE_CURVE ( 'NONE', #16594, #7151, #25481, .T. ) ;
#8156 = CARTESIAN_POINT ( 'NONE',  ( 33.31606138205700773, 3.536347952325769040, 64.10938348997790115 ) ) ;
#8157 = CARTESIAN_POINT ( 'NONE',  ( 38.26194895904384197, -20.60384086642191193, 72.51602215082118619 ) ) ;
#8158 = ADVANCED_FACE ( 'NONE', ( #12524 ), #23829, .T. ) ;
#8159 = EDGE_CURVE ( 'NONE', #13577, #25244, #20362, .T. ) ;
#8160 = EDGE_LOOP ( 'NONE', ( #23217, #22905, #15243, #4859 ) ) ;
#8161 = ORIENTED_EDGE ( 'NONE', *, *, #14678, .F. ) ;
#8162 = FACE_OUTER_BOUND ( 'NONE', #5613, .T. ) ;
#8163 = CARTESIAN_POINT ( 'NONE',  ( 40.31606138205700773, -26.06829118875199924, 75.30501292736998664 ) ) ;
#8164 = CARTESIAN_POINT ( 'NONE',  ( 38.26194895904384197, -22.60384086642191903, 73.71602215082113219 ) ) ;
#8165 = AXIS2_PLACEMENT_3D ( 'NONE', #970, #19019, #1095 ) ;
#8166 = VECTOR ( 'NONE', #5362, 1000.000000000000000 ) ;
#8167 = FACE_OUTER_BOUND ( 'NONE', #3413, .T. ) ;
#8168 = CARTESIAN_POINT ( 'NONE',  ( 37.25202387243752611, -25.21368208888610241, 70.00779233799262613 ) ) ;
#8169 = EDGE_CURVE ( 'NONE', #23532, #20004, #8254, .T. ) ;
#8170 = CARTESIAN_POINT ( 'NONE',  ( 43.06606138205700063, 42.19123852234599781, 74.30501292736987295 ) ) ;
#8171 = ADVANCED_FACE ( 'NONE', ( #14057 ), #21910, .T. ) ;
#8172 = ORIENTED_EDGE ( 'NONE', *, *, #3284, .T. ) ;
#8173 = PLANE ( 'NONE',  #20724 ) ;
#8174 = FACE_OUTER_BOUND ( 'NONE', #11170, .T. ) ;
#8175 = CARTESIAN_POINT ( 'NONE',  ( 39.95015449827720744, -21.00384086642191406, 71.96809898377887293 ) ) ;
#8176 = CARTESIAN_POINT ( 'NONE',  ( 45.81606138205700063, -34.67340937580780036, 71.26505871168839690 ) ) ;
#8177 = AXIS2_PLACEMENT_3D ( 'NONE', #12636, #15761, #21567 ) ;
#8178 = EDGE_LOOP ( 'NONE', ( #14701, #6163, #4835, #18166 ) ) ;
#8179 = CARTESIAN_POINT ( 'NONE',  ( 32.56606138205700773, 40.39281886181299797, 82.55501292736983032 ) ) ;
#8180 = DIRECTION ( 'NONE',  ( -2.011972697750612571E-15, 0.6595716529892353686, -0.7516416929448815898 ) ) ;
#8181 = CARTESIAN_POINT ( 'NONE',  ( 39.37952058850012804, 0.9961591335780894951, 71.78268878715394408 ) ) ;
#8182 = DIRECTION ( 'NONE',  ( -1.000000000000000000, 0.000000000000000000, 0.000000000000000000 ) ) ;
#8183 = EDGE_LOOP ( 'NONE', ( #18540, #20030, #23817, #7613, #6063, #23031, #7421, #3796, #12314, #14967, #16575, #22904, #435, #1746, #14732, #15175, #19822, #24588, #9971 ) ) ;
#8184 = VECTOR ( 'NONE', #16023, 1000.000000000000000 ) ;
#8185 = DIRECTION ( 'NONE',  ( 0.000000000000000000, 0.6595716529892354796, -0.7516416929448814788 ) ) ;
#8186 = ORIENTED_EDGE ( 'NONE', *, *, #554, .F. ) ;
#8187 = ORIENTED_EDGE ( 'NONE', *, *, #3529, .F. ) ;
#8188 = CARTESIAN_POINT ( 'NONE',  ( 36.31606138205700773, -20.93502329652820038, 27.89939821807130826 ) ) ;
#8189 = DIRECTION ( 'NONE',  ( -1.000000000000000000, 0.000000000000000000, 0.000000000000000000 ) ) ;
#8190 = CARTESIAN_POINT ( 'NONE',  ( 37.21915885897815457, -5.413682088886103472, 71.08074471024443142 ) ) ;
#8191 = AXIS2_PLACEMENT_3D ( 'NONE', #15192, #23295, #15574 ) ;
#8192 = CARTESIAN_POINT ( 'NONE',  ( 37.89291511884476904, -3.113682088886100097, 70.26206559358664094 ) ) ;
#8193 = ORIENTED_EDGE ( 'NONE', *, *, #12417, .T. ) ;
#8194 = ORIENTED_EDGE ( 'NONE', *, *, #6841, .T. ) ;
#8195 = PLANE ( 'NONE',  #18147 ) ;
#8196 = FACE_BOUND ( 'NONE', #17765, .T. ) ;
#8197 = EDGE_LOOP ( 'NONE', ( #8999, #19174, #8977, #17273 ) ) ;
#8198 = DIRECTION ( 'NONE',  ( 6.505213034913089466E-17, -1.000000000000000000, 3.491481338843135327E-15 ) ) ;
#8199 = CARTESIAN_POINT ( 'NONE',  ( 39.38009889167648936, -13.40384086642191086, 70.00779233799262613 ) ) ;
#8200 = VECTOR ( 'NONE', #3454, 1000.000000000000227 ) ;
#8201 = CARTESIAN_POINT ( 'NONE',  ( 36.72121174906109786, -21.47489429109494807, 75.83882253612472368 ) ) ;
#8202 = DIRECTION ( 'NONE',  ( 1.000000000000000000, 0.000000000000000000, -0.000000000000000000 ) ) ;
#8203 = VERTEX_POINT ( 'NONE', #4273 ) ;
#8204 = AXIS2_PLACEMENT_3D ( 'NONE', #18682, #3340, #11217 ) ;
#8205 = ORIENTED_EDGE ( 'NONE', *, *, #19252, .T. ) ;
#8206 = AXIS2_PLACEMENT_3D ( 'NONE', #2960, #4907, #10586 ) ;
#8207 = LINE ( 'NONE', #10393, #2572 ) ;
#8208 = CARTESIAN_POINT ( 'NONE',  ( 38.93415946300898867, -6.113682088886108090, 73.09843995877331224 ) ) ;
#8209 = LINE ( 'NONE', #12210, #735 ) ;
#8210 = DIRECTION ( 'NONE',  ( -8.758115402030106693E-47, 1.000000000000000000, -3.469446951953613400E-15 ) ) ;
#8211 = VECTOR ( 'NONE', #461, 999.9999999999998863 ) ;
#8212 = FACE_OUTER_BOUND ( 'NONE', #17272, .T. ) ;
#8213 = CARTESIAN_POINT ( 'NONE',  ( 36.31606138205700063, 38.69123852234599070, 73.55501292736988717 ) ) ;
#8214 = CIRCLE ( 'NONE', #14387, 12.59999999999999964 ) ;
#8215 = LINE ( 'NONE', #14264, #16013 ) ;
#8216 = LINE ( 'NONE', #18141, #5272 ) ;
#8217 = VECTOR ( 'NONE', #855, 1000.000000000000000 ) ;
#8218 = VERTEX_POINT ( 'NONE', #2569 ) ;
#8219 = DIRECTION ( 'NONE',  ( 0.000000000000000000, -3.491481338843135327E-15, -1.000000000000000000 ) ) ;
#8220 = ORIENTED_EDGE ( 'NONE', *, *, #12827, .T. ) ;
#8221 = VERTEX_POINT ( 'NONE', #12643 ) ;
#8222 = CARTESIAN_POINT ( 'NONE',  ( 41.31606138205700063, 1.535676793533870210, 63.36117568837578062 ) ) ;
#8223 = CARTESIAN_POINT ( 'NONE',  ( 39.12911128074872380, -7.503840866421911393, 69.06206559358666652 ) ) ;
#8224 = CIRCLE ( 'NONE', #17261, 0.4999999999999982792 ) ;
#8225 = EDGE_LOOP ( 'NONE', ( #20569, #20634, #22497, #2, #10807 ) ) ;
#8226 = LINE ( 'NONE', #24165, #16523 ) ;
#8227 = CARTESIAN_POINT ( 'NONE',  ( 39.82603832034400426, -6.313682088886107380, 72.40698646996135324 ) ) ;
#8228 = AXIS2_PLACEMENT_3D ( 'NONE', #10761, #3001, #22848 ) ;
#8229 = EDGE_LOOP ( 'NONE', ( #19877, #7367, #16833, #18895 ) ) ;
#8230 = LINE ( 'NONE', #14404, #1744 ) ;
#8231 = CARTESIAN_POINT ( 'NONE',  ( 40.52078840805428683, -12.61368208888610454, 70.60699637195608602 ) ) ;
#8232 = VECTOR ( 'NONE', #10753, 1000.000000000000000 ) ;
#8233 = CARTESIAN_POINT ( 'NONE',  ( 38.31606138205700063, 42.51966564709218233, 71.30501292737018559 ) ) ;
#8234 = VECTOR ( 'NONE', #19466, 1000.000000000000000 ) ;
#8235 = ADVANCED_FACE ( 'NONE', ( #19983 ), #18055, .F. ) ;
#8236 = CARTESIAN_POINT ( 'NONE',  ( 42.82259893474252266, 3.224890024296139135, 6.370941811568299862 ) ) ;
#8237 =( NAMED_UNIT ( * ) SI_UNIT ( $, .STERADIAN. ) SOLID_ANGLE_UNIT ( ) );
#8238 = ADVANCED_FACE ( 'NONE', ( #8261 ), #2442, .F. ) ;
#8239 = CARTESIAN_POINT ( 'NONE',  ( 43.81606138205700063, 3.151453266960317023, 6.397347472316774031 ) ) ;
#8240 = CARTESIAN_POINT ( 'NONE',  ( 41.31606138205700063, 1.207247317117632335, 63.73818242441765847 ) ) ;
#8241 = PLANE ( 'NONE',  #7793 ) ;
#8242 = CARTESIAN_POINT ( 'NONE',  ( 39.02742774030102879, -22.21368208888610241, 72.26730301774234988 ) ) ;
#8243 = VERTEX_POINT ( 'NONE', #14309 ) ;
#8244 = VECTOR ( 'NONE', #25240, 1000.000000000000000 ) ;
#8245 = CARTESIAN_POINT ( 'NONE',  ( 38.96215273200666473, -22.11862185030787842, 75.30541206002871490 ) ) ;
#8246 = CARTESIAN_POINT ( 'NONE',  ( 45.81606138205700063, 44.92314894770294131, 81.17823623207320338 ) ) ;
#8247 = ORIENTED_EDGE ( 'NONE', *, *, #17847, .T. ) ;
#8248 = ORIENTED_EDGE ( 'NONE', *, *, #22157, .F. ) ;
#8249 = UNCERTAINTY_MEASURE_WITH_UNIT (LENGTH_MEASURE( 1.000000000000000082E-05 ), #2358, 'distance_accuracy_value', 'NONE');
#8250 = CIRCLE ( 'NONE', #9925, 0.9023161253044892360 ) ;
#8251 = CARTESIAN_POINT ( 'NONE',  ( 39.73277004305197124, -23.40384086642191264, 69.52238214136768590 ) ) ;
#8252 = ADVANCED_FACE ( 'NONE', ( #16236 ), #22158, .T. ) ;
#8253 = CARTESIAN_POINT ( 'NONE',  ( 36.80608444377001121, -25.31368208888610383, 70.35351908239857721 ) ) ;
#8254 = CIRCLE ( 'NONE', #25081, 0.7499999999999983347 ) ;
#8255 = DIRECTION ( 'NONE',  ( 0.1803747433772539821, 0.9835979625596982245, 0.000000000000000000 ) ) ;
#8256 = DIRECTION ( 'NONE',  ( 0.000000000000000000, -6.938893903907222067E-15, 1.000000000000000000 ) ) ;
#8257 = VERTEX_POINT ( 'NONE', #24956 ) ;
#8258 = DIRECTION ( 'NONE',  ( -1.734723475976814737E-16, 0.000000000000000000, -1.000000000000000000 ) ) ;
#8259 = CARTESIAN_POINT ( 'NONE',  ( 34.06606138205700773, -39.60075215179220720, 69.23691647014479145 ) ) ;
#8260 = CARTESIAN_POINT ( 'NONE',  ( 37.61123632939164452, -1.703840866421911571, 69.02690120949094421 ) ) ;
#8261 = FACE_OUTER_BOUND ( 'NONE', #7636, .T. ) ;
#8262 = DIRECTION ( 'NONE',  ( -1.000000000000000000, 0.000000000000000000, 0.000000000000000000 ) ) ;
#8263 = CARTESIAN_POINT ( 'NONE',  ( 38.93415946300897446, -10.11368208888610987, 73.09843995877331224 ) ) ;
#8264 = DIRECTION ( 'NONE',  ( 0.000000000000000000, 1.000000000000000000, -2.999999999999999839E-15 ) ) ;
#8265 = AXIS2_PLACEMENT_3D ( 'NONE', #17796, #23822, #127 ) ;
#8266 = MANIFOLD_SOLID_BREP ( 'NONE', #2752 ) ;
#8267 = CARTESIAN_POINT ( 'NONE',  ( 36.64852494920107517, -27.41368208888610525, 70.89533451361945993 ) ) ;
#8268 = CIRCLE ( 'NONE', #2489, 2.000000000000000000 ) ;
#8269 = DIRECTION ( 'NONE',  ( 1.000000000000000000, -6.938893903907222067E-15, 0.000000000000000000 ) ) ;
#8270 = DIRECTION ( 'NONE',  ( -0.000000000000000000, -3.469446951953613400E-15, -1.000000000000000000 ) ) ;
#8271 = ITEM_DEFINED_TRANSFORMATION ( 'NONE', 'NONE', #16229,  #2000 ) ;
#8272 = DIRECTION ( 'NONE',  ( -1.000000000000000000, -2.870367030604242092E-15, 6.397632838472598363E-17 ) ) ;
#8273 = CARTESIAN_POINT ( 'NONE',  ( 37.69225076346193504, -27.80384086642191477, 70.42958956619166599 ) ) ;
#8274 = CARTESIAN_POINT ( 'NONE',  ( 39.82603832034400426, -14.31368208888610916, 72.40698646996133903 ) ) ;
#8275 = CARTESIAN_POINT ( 'NONE',  ( 40.56606138205695089, 4.754708485422523445, 4.090082623941899698 ) ) ;
#8276 = CARTESIAN_POINT ( 'NONE',  ( 39.38009889167648936, -13.40384086642191086, 70.00779233799262613 ) ) ;
#8277 = CYLINDRICAL_SURFACE ( 'NONE', #7284, 1.749999999999999778 ) ;
#8278 = EDGE_CURVE ( 'NONE', #5334, #18694, #24710, .T. ) ;
#8279 = CARTESIAN_POINT ( 'NONE',  ( 39.82603832034400426, -12.31368208888610560, 72.40698646996133903 ) ) ;
#8280 = ORIENTED_EDGE ( 'NONE', *, *, #8581, .T. ) ;
#8281 = CARTESIAN_POINT ( 'NONE',  ( 36.98690846071097837, -15.81368208888610916, 73.30173637941818754 ) ) ;
#8282 = ORIENTED_EDGE ( 'NONE', *, *, #5603, .T. ) ;
#8283 = DIRECTION ( 'NONE',  ( 0.000000000000000000, -0.7540134720837717852, -0.6568589528324746407 ) ) ;
#8284 = B_SPLINE_CURVE_WITH_KNOTS ( 'NONE', 3,
 ( #3913, #4035, #7656, #5716, #163, #12039, #17320, #1837, #11909, #15881, #13579, #19499, #23736, #19370 ),
 .UNSPECIFIED., .F., .F.,
 ( 4, 2, 2, 2, 2, 2, 4 ),
 ( 0.0007428411354317481169, 0.0009550568131542710483, 0.001167272490876794088, 0.001273380329738076858, 0.001379488168599359195, 0.001485596007460641965, 0.001591703846321924519 ),
 .UNSPECIFIED. ) ;
#8285 = CARTESIAN_POINT ( 'NONE',  ( 31.81606138205700418, 35.44123852234597649, 68.30501292736990138 ) ) ;
#8286 = AXIS2_PLACEMENT_3D ( 'NONE', #1873, #13487, #9638 ) ;
#8287 = CARTESIAN_POINT ( 'NONE',  ( 39.37952058850012804, -17.00384086642191406, 71.78268878715390144 ) ) ;
#8288 = ORIENTED_EDGE ( 'NONE', *, *, #1251, .F. ) ;
#8289 = ORIENTED_EDGE ( 'NONE', *, *, #2231, .F. ) ;
#8290 = LINE ( 'NONE', #6478, #2238 ) ;
#8291 = LINE ( 'NONE', #12292, #12497 ) ;
#8292 = CARTESIAN_POINT ( 'NONE',  ( 38.37017380507018771, -23.60384086642191903, 69.04448340153878405 ) ) ;
#8293 = CARTESIAN_POINT ( 'NONE',  ( 40.64099152588522657, 1.832818861813001021, 78.30501292736998664 ) ) ;
#8294 = CARTESIAN_POINT ( 'NONE',  ( 39.02088643472237095, 1.086317911113899415, 69.02690120949095842 ) ) ;
#8295 = PRODUCT_DEFINITION_SHAPE ( 'NONE', 'NONE',  #25492 ) ;
#8296 = DIRECTION ( 'NONE',  ( 1.000000000000000000, 1.734723475976814737E-16, -1.734723475976804876E-16 ) ) ;
#8297 = ADVANCED_FACE ( 'NONE', ( #7219 ), #9162, .F. ) ;
#8298 = ORIENTED_EDGE ( 'NONE', *, *, #22816, .T. ) ;
#8299 = LINE ( 'NONE', #11921, #13740 ) ;
#8300 = EDGE_CURVE ( 'NONE', #10990, #6757, #10828, .T. ) ;
#8301 = CARTESIAN_POINT ( 'NONE',  ( 38.31606138205700063, 39.69123852234599070, 72.30501292737018559 ) ) ;
#8302 = CARTESIAN_POINT ( 'NONE',  ( 39.82603832034401137, -21.30384086642191122, 70.35351908239857721 ) ) ;
#8303 = ADVANCED_FACE ( 'NONE', ( #14810, #5409, #882 ), #1409, .T. ) ;
#8304 =( LENGTH_UNIT ( ) NAMED_UNIT ( * ) SI_UNIT ( .MILLI., .METRE. ) );
#8305 = DIRECTION ( 'NONE',  ( 1.000000000000000000, 0.000000000000000000, 0.000000000000000000 ) ) ;
#8306 = EDGE_CURVE ( 'NONE', #17348, #6502, #22916, .T. ) ;
#8307 = EDGE_CURVE ( 'NONE', #5367, #4383, #13147, .T. ) ;
#8308 = DIRECTION ( 'NONE',  ( 0.000000000000000000, 0.000000000000000000, -1.000000000000000000 ) ) ;
#8309 = PRESENTATION_LAYER_ASSIGNMENT (  '', '', ( #9146 ) ) ;
#8310 = LINE ( 'NONE', #15780, #20549 ) ;
#8311 = CARTESIAN_POINT ( 'NONE',  ( 39.37952058850012804, -3.003840866421910505, 71.78268878715392987 ) ) ;
#8312 = DIRECTION ( 'NONE',  ( -3.083952846180990083E-15, 1.000000000000000000, -2.999999999999998655E-15 ) ) ;
#8313 = ORIENTED_EDGE ( 'NONE', *, *, #18260, .T. ) ;
#8314 = ADVANCED_FACE ( 'NONE', ( #10952 ), #20616, .T. ) ;
#8315 = LINE ( 'NONE', #17860, #22257 ) ;
#8316 = ORIENTED_EDGE ( 'NONE', *, *, #5079, .T. ) ;
#8317 = VERTEX_POINT ( 'NONE', #8776 ) ;
#8318 = DIRECTION ( 'NONE',  ( 0.000000000000000000, 1.000000000000000000, -2.999999999999998655E-15 ) ) ;
#8319 = CARTESIAN_POINT ( 'NONE',  ( 32.31606138205700063, -20.55619265724211076, 44.11584019928223910 ) ) ;
#8320 = CARTESIAN_POINT ( 'NONE',  ( 38.37017380507020192, -4.013682088886100452, 72.51602215082118619 ) ) ;
#8321 = CARTESIAN_POINT ( 'NONE',  ( 37.69225076346193504, -7.813682088886102939, 72.33091598616827866 ) ) ;
#8322 = ORIENTED_EDGE ( 'NONE', *, *, #17911, .F. ) ;
#8323 = ORIENTED_EDGE ( 'NONE', *, *, #16079, .T. ) ;
#8324 = DIRECTION ( 'NONE',  ( -1.000000000000000000, -2.556434596176347380E-15, -1.460819769243627131E-15 ) ) ;
#8325 = CARTESIAN_POINT ( 'NONE',  ( 46.81606138205707879, -39.09901169483115524, 63.57464975149190423 ) ) ;
#8326 = FACE_OUTER_BOUND ( 'NONE', #24275, .T. ) ;
#8327 = VECTOR ( 'NONE', #3815, 1000.000000000000000 ) ;
#8328 = CARTESIAN_POINT ( 'NONE',  ( 38.26194895904384907, -10.60384086642191726, 73.11602215082118050 ) ) ;
#8329 = AXIS2_PLACEMENT_3D ( 'NONE', #8357, #16447, #10793 ) ;
#8330 =( REPRESENTATION_RELATIONSHIP ('NONE','NONE', #17377, #11141 ) REPRESENTATION_RELATIONSHIP_WITH_TRANSFORMATION ( #14199 )SHAPE_REPRESENTATION_RELATIONSHIP( ) );
#8331 = CARTESIAN_POINT ( 'NONE',  ( 40.31606138205699352, -9.599063827782591929, 29.78523791026437095 ) ) ;
#8332 = DIRECTION ( 'NONE',  ( 0.000000000000000000, 2.775557561562888984E-15, 1.000000000000000000 ) ) ;
#8333 = AXIS2_PLACEMENT_3D ( 'NONE', #7177, #24916, #12849 ) ;
#8334 = CARTESIAN_POINT ( 'NONE',  ( 36.31606138205700773, -21.38339321089542722, 27.67811916372966863 ) ) ;
#8335 = ORIENTED_EDGE ( 'NONE', *, *, #3252, .T. ) ;
#8336 = ORIENTED_EDGE ( 'NONE', *, *, #6319, .F. ) ;
#8337 = ORIENTED_EDGE ( 'NONE', *, *, #4215, .T. ) ;
#8338 = LINE ( 'NONE', #23780, #17411 ) ;
#8339 = CARTESIAN_POINT ( 'NONE',  ( 38.93415946300898867, -10.11368208888610987, 73.09843995877331224 ) ) ;
#8340 = DIRECTION ( 'NONE',  ( -1.000000000000000000, 3.491481338843135327E-15, -1.047444401652940473E-29 ) ) ;
#8341 = CARTESIAN_POINT ( 'NONE',  ( 33.66606138205698073, -5.898435835062239008, -2.003809078978638247 ) ) ;
#8342 = EDGE_CURVE ( 'NONE', #24513, #6624, #16398, .T. ) ;
#8343 = ADVANCED_FACE ( 'NONE', ( #13273 ), #9295, .T. ) ;
#8344 = LINE ( 'NONE', #8089, #3217 ) ;
#8345 = AXIS2_PLACEMENT_3D ( 'NONE', #23275, #9649, #3450 ) ;
#8346 = DIRECTION ( 'NONE',  ( 0.000000000000000000, 0.000000000000000000, 1.000000000000000000 ) ) ;
#8347 = CARTESIAN_POINT ( 'NONE',  ( 40.31606138205700773, 37.94123852234599070, 73.55501292736988717 ) ) ;
#8348 = AXIS2_PLACEMENT_3D ( 'NONE', #2879, #3402, #5345 ) ;
#8349 = EDGE_CURVE ( 'NONE', #21215, #22719, #20528, .T. ) ;
#8350 = LINE ( 'NONE', #4355, #2913 ) ;
#8351 = ORIENTED_EDGE ( 'NONE', *, *, #9974, .F. ) ;
#8352 = ORIENTED_EDGE ( 'NONE', *, *, #18529, .T. ) ;
#8353 = PLANE ( 'NONE',  #18198 ) ;
#8354 = CARTESIAN_POINT ( 'NONE',  ( 38.26194895904384197, -4.603840866421918143, 73.71602215082116061 ) ) ;
#8355 = EDGE_LOOP ( 'NONE', ( #4592, #18766, #20672, #16551 ) ) ;
#8356 = AXIS2_PLACEMENT_3D ( 'NONE', #16981, #13121, #5137 ) ;
#8357 = CARTESIAN_POINT ( 'NONE',  ( 32.56606138205700773, 41.41058581477939526, 84.01211970855638356 ) ) ;
#8358 = CARTESIAN_POINT ( 'NONE',  ( 39.82603832034400426, -8.313682088886110932, 72.40698646996135324 ) ) ;
#8359 = AXIS2_PLACEMENT_3D ( 'NONE', #8612, #8743, #12859 ) ;
#8360 = CARTESIAN_POINT ( 'NONE',  ( 43.81606138205700063, -25.26124097814961544, 70.06813202641110649 ) ) ;
#8361 = ADVANCED_FACE ( 'NONE', ( #13017, #4894 ), #9790, .T. ) ;
#8362 = AXIS2_PLACEMENT_3D ( 'NONE', #16256, #12165, #14215 ) ;
#8363 = CARTESIAN_POINT ( 'NONE',  ( 35.86008812008917346, -15.51368208888610667, 71.43714994484034264 ) ) ;
#8364 = AXIS2_PLACEMENT_3D ( 'NONE', #13466, #23494, #22992 ) ;
#8365 = DIRECTION ( 'NONE',  ( -4.336808689942015271E-16, 4.914813388431354887E-16, -1.000000000000000000 ) ) ;
#8366 = DIRECTION ( 'NONE',  ( 0.000000000000000000, 1.000000000000000000, 1.632680918566405215E-15 ) ) ;
#8367 = AXIS2_PLACEMENT_3D ( 'NONE', #15123, #4824, #9346 ) ;
#8368 = DIRECTION ( 'NONE',  ( 0.000000000000000000, 0.7540134720837717852, 0.6568589528324745297 ) ) ;
#8369 = FACE_OUTER_BOUND ( 'NONE', #2459, .T. ) ;
#8370 = CIRCLE ( 'NONE', #11246, 0.5000000000000004441 ) ;
#8371 = CARTESIAN_POINT ( 'NONE',  ( 35.31606138205687273, 42.19123852234599781, 75.30501292736987295 ) ) ;
#8372 = DIRECTION ( 'NONE',  ( 2.792262043613788141E-15, -0.8967398287344626739, -0.4425581086832399147 ) ) ;
#8373 = CARTESIAN_POINT ( 'NONE',  ( 38.93987200065208754, -26.81368208888610738, 70.42958956619166599 ) ) ;
#8374 = ORIENTED_EDGE ( 'NONE', *, *, #7554, .T. ) ;
#8375 = PRESENTATION_LAYER_ASSIGNMENT (  '', '', ( #17014 ) ) ;
#8376 = CARTESIAN_POINT ( 'NONE',  ( 40.31606138205700773, -30.30876147765400574, 73.55501292737010033 ) ) ;
#8377 = LINE ( 'NONE', #16219, #7441 ) ;
#8378 = ORIENTED_EDGE ( 'NONE', *, *, #3932, .T. ) ;
#8379 = ORIENTED_EDGE ( 'NONE', *, *, #11831, .T. ) ;
#8380 = AXIS2_PLACEMENT_3D ( 'NONE', #2731, #14984, #14598 ) ;
#8381 = CARTESIAN_POINT ( 'NONE',  ( 35.86008812008917346, -26.10384086642191903, 71.32335560751960202 ) ) ;
#8382 = AXIS2_PLACEMENT_3D ( 'NONE', #10448, #15971, #24079 ) ;
#8383 = CARTESIAN_POINT ( 'NONE',  ( 39.02088643472237095, 1.086317911113899415, 69.02690120949095842 ) ) ;
#8384 = CARTESIAN_POINT ( 'NONE',  ( 40.31606138205700773, -19.47805968271054766, 24.94720442500192448 ) ) ;
#8385 = EDGE_CURVE ( 'NONE', #14366, #12562, #20129, .T. ) ;
#8386 = EDGE_CURVE ( 'NONE', #19553, #8450, #7603, .T. ) ;
#8387 = FACE_OUTER_BOUND ( 'NONE', #23235, .T. ) ;
#8388 = CARTESIAN_POINT ( 'NONE',  ( 38.31606138205700063, -29.78523130861184143, 52.92072663988442116 ) ) ;
#8389 = ORIENTED_EDGE ( 'NONE', *, *, #18706, .F. ) ;
#8390 = AXIS2_PLACEMENT_3D ( 'NONE', #17083, #9236, #21069 ) ;
#8391 = CARTESIAN_POINT ( 'NONE',  ( 45.81606138205694378, 5.290470704224633280, -0.3848988112044732235 ) ) ;
#8392 = DIRECTION ( 'NONE',  ( 1.000000000000000000, 0.000000000000000000, 0.000000000000000000 ) ) ;
#8393 = CARTESIAN_POINT ( 'NONE',  ( 36.29569395875881099, -2.303840866421917877, 72.77780686321129622 ) ) ;
#8394 = DIRECTION ( 'NONE',  ( 1.000000000000000000, 0.000000000000000000, 0.000000000000000000 ) ) ;
#8395 = PLANE ( 'NONE',  #17766 ) ;
#8396 = CARTESIAN_POINT ( 'NONE',  ( 38.82593461698262871, -6.913682088886100807, 69.62690120949091011 ) ) ;
#8397 = LINE ( 'NONE', #16239, #7252 ) ;
#8398 = MANIFOLD_SOLID_BREP ( 'NONE', #6484 ) ;
#8399 = CARTESIAN_POINT ( 'NONE',  ( 40.14115730948191185, -28.51368208888610667, 71.32335560751960202 ) ) ;
#8400 = AXIS2_PLACEMENT_3D ( 'NONE', #7347, #21252, #11091 ) ;
#8401 = CARTESIAN_POINT ( 'NONE',  ( 36.31606138205700063, -11.18542543036242343, 17.47151328161626793 ) ) ;
#8402 = EDGE_CURVE ( 'NONE', #5555, #11300, #16808, .T. ) ;
#8403 = VECTOR ( 'NONE', #21245, 1000.000000000000000 ) ;
#8404 = DIRECTION ( 'NONE',  ( 0.000000000000000000, -1.000000000000000000, 0.000000000000000000 ) ) ;
#8405 = CARTESIAN_POINT ( 'NONE',  ( 39.37952058850012804, -23.00384086642191050, 71.78268878715390144 ) ) ;
#8406 = CARTESIAN_POINT ( 'NONE',  ( 39.75915168707250302, -12.71368208888610063, 70.26145752964251301 ) ) ;
#8407 = DIRECTION ( 'NONE',  ( 0.000000000000000000, -0.7540134720837697868, -0.6568589528324768612 ) ) ;
#8408 = CARTESIAN_POINT ( 'NONE',  ( 39.95015449827720744, -11.00384086642191050, 71.96809898377888715 ) ) ;
#8409 = CARTESIAN_POINT ( 'NONE',  ( 31.56606138205707879, -39.99575152356569419, 63.13209164280871022 ) ) ;
#8410 =( GEOMETRIC_REPRESENTATION_CONTEXT ( 3 ) GLOBAL_UNCERTAINTY_ASSIGNED_CONTEXT ( ( #18793 ) ) GLOBAL_UNIT_ASSIGNED_CONTEXT ( ( #11924, #1975, #46 ) ) REPRESENTATION_CONTEXT ( 'NONE', 'WORKASPACE' ) );
#8411 = CARTESIAN_POINT ( 'NONE',  ( 39.98359781491296161, -14.41368208888610525, 71.86517103874047052 ) ) ;
#8412 = VERTEX_POINT ( 'NONE', #17386 ) ;
#8413 = CARTESIAN_POINT ( 'NONE',  ( 36.29569395875879678, -13.31368208888610205, 69.98269868914867686 ) ) ;
#8414 = ORIENTED_EDGE ( 'NONE', *, *, #17520, .T. ) ;
#8415 = CARTESIAN_POINT ( 'NONE',  ( 43.81606138205700063, 41.44123852234596939, 66.30501292736988717 ) ) ;
#8416 = AXIS2_PLACEMENT_3D ( 'NONE', #4681, #12557, #437 ) ;
#8417 = FACE_BOUND ( 'NONE', #25472, .T. ) ;
#8418 = CARTESIAN_POINT ( 'NONE',  ( 39.51027997493896748, -19.10384086642191193, 71.43714994484032843 ) ) ;
#8419 = ORIENTED_EDGE ( 'NONE', *, *, #14782, .F. ) ;
#8420 = ORIENTED_EDGE ( 'NONE', *, *, #7580, .T. ) ;
#8421 = DIRECTION ( 'NONE',  ( 0.000000000000000000, 2.999999999999999839E-15, 1.000000000000000000 ) ) ;
#8422 = STYLED_ITEM ( 'NONE', ( #11915 ), #16907 ) ;
#8423 = CARTESIAN_POINT ( 'NONE',  ( 30.81606138205700418, -34.67340937580780036, 71.26505871168839690 ) ) ;
#8424 = CARTESIAN_POINT ( 'NONE',  ( 39.73277004305197124, -25.40384086642191264, 69.52238214136765748 ) ) ;
#8425 = CARTESIAN_POINT ( 'NONE',  ( 44.81606138205700063, -38.55876147765401640, 71.30501292737012875 ) ) ;
#8426 = CARTESIAN_POINT ( 'NONE',  ( 39.29254315202756231, -24.81368208888610383, 69.94417936956671156 ) ) ;
#8427 = CYLINDRICAL_SURFACE ( 'NONE', #1539, 0.7500000000000022204 ) ;
#8428 = VERTEX_POINT ( 'NONE', #3850 ) ;
#8429 = DIRECTION ( 'NONE',  ( 1.000000000000000000, -0.000000000000000000, 0.000000000000000000 ) ) ;
#8430 = AXIS2_PLACEMENT_3D ( 'NONE', #20655, #672, #14721 ) ;
#8431 = CARTESIAN_POINT ( 'NONE',  ( 33.80827534892208064, -20.02093502212017029, 26.61211107664843212 ) ) ;
#8432 = ADVANCED_FACE ( 'NONE', ( #17258, #3714, #1521, #1779 ), #5919, .F. ) ;
#8433 = CARTESIAN_POINT ( 'NONE',  ( 39.98359781491296161, -13.20384086642191157, 70.89533451361945993 ) ) ;
#8434 = VECTOR ( 'NONE', #10102, 1000.000000000000000 ) ;
#8435 = CARTESIAN_POINT ( 'NONE',  ( 40.81606138205700063, 5.691238522346998785, 68.80501292736998664 ) ) ;
#8436 = DIRECTION ( 'NONE',  ( 1.000000000000000000, 0.000000000000000000, 0.000000000000000000 ) ) ;
#8437 = DIRECTION ( 'NONE',  ( -1.000000000000000000, -1.208430656372714685E-15, -2.875977885193763990E-16 ) ) ;
#8438 = CARTESIAN_POINT ( 'NONE',  ( 36.49096545463212493, -28.10384086642190127, 71.32335560751960202 ) ) ;
#8439 = CARTESIAN_POINT ( 'NONE',  ( 38.31606138205700773, -22.27515649656512053, 29.48506754039017963 ) ) ;
#8440 = VERTEX_POINT ( 'NONE', #11732 ) ;
#8441 = DIRECTION ( 'NONE',  ( 1.000000000000000000, 0.000000000000000000, 0.000000000000000000 ) ) ;
#8442 = VERTEX_POINT ( 'NONE', #9671 ) ;
#8443 = ORIENTED_EDGE ( 'NONE', *, *, #4601, .F. ) ;
#8444 = CYLINDRICAL_SURFACE ( 'NONE', #19728, 0.5000000000000004441 ) ;
#8445 = CARTESIAN_POINT ( 'NONE',  ( 44.31606138205700063, -20.93319939328399926, 43.78741072286599945 ) ) ;
#8446 = UNCERTAINTY_MEASURE_WITH_UNIT (LENGTH_MEASURE( 1.000000000000000082E-05 ), #22278, 'distance_accuracy_value', 'NONE');
#8447 = CARTESIAN_POINT ( 'NONE',  ( 39.41296390513587511, -4.413682088886102584, 71.67976084211552745 ) ) ;
#8448 = EDGE_CURVE ( 'NONE', #12300, #25398, #11347, .T. ) ;
#8449 = CARTESIAN_POINT ( 'NONE',  ( 39.31564783533280405, -2.313682088886100718, 72.03616607671141026 ) ) ;
#8450 = VERTEX_POINT ( 'NONE', #3589 ) ;
#8451 = ORIENTED_EDGE ( 'NONE', *, *, #19820, .T. ) ;
#8452 = LINE ( 'NONE', #20168, #20595 ) ;
#8453 = CARTESIAN_POINT ( 'NONE',  ( 43.81606138205700063, 35.12314894770293705, 81.17823623207323180 ) ) ;
#8454 = ORIENTED_EDGE ( 'NONE', *, *, #7135, .F. ) ;
#8455 = CARTESIAN_POINT ( 'NONE',  ( 31.81606138205700418, -34.55876147765410167, 70.30501292737000085 ) ) ;
#8456 = CARTESIAN_POINT ( 'NONE',  ( 39.75915168707251723, -12.90384086642191797, 72.49904802271738902 ) ) ;
#8457 = EDGE_CURVE ( 'NONE', #2232, #2532, #23167, .T. ) ;
#8458 = CARTESIAN_POINT ( 'NONE',  ( 44.71606138205697079, -4.349482454670842380, -5.142398479549302515 ) ) ;
#8459 = DIRECTION ( 'NONE',  ( 0.000000000000000000, 0.000000000000000000, 1.000000000000000000 ) ) ;
#8460 = VERTEX_POINT ( 'NONE', #2039 ) ;
#8461 = VERTEX_POINT ( 'NONE', #13778 ) ;
#8462 = ORIENTED_EDGE ( 'NONE', *, *, #24940, .F. ) ;
#8463 = DIRECTION ( 'NONE',  ( 1.000000000000000000, -0.000000000000000000, 0.000000000000000000 ) ) ;
#8464 = CARTESIAN_POINT ( 'NONE',  ( 38.26194895904383486, -7.013682088886100452, 69.64448340153879258 ) ) ;
#8465 = EDGE_CURVE ( 'NONE', #22735, #18487, #1989, .T. ) ;
#8466 = CARTESIAN_POINT ( 'NONE',  ( 40.03626012656804534, -29.10876147765398159, 71.40821190666599705 ) ) ;
#8467 = PLANE ( 'NONE',  #17815 ) ;
#8468 = CARTESIAN_POINT ( 'NONE',  ( 37.69796330110504101, -27.11368208888609388, 69.66206559358660400 ) ) ;
#8469 = CARTESIAN_POINT ( 'NONE',  ( 39.76930122830209058, -29.10876147765397803, 69.95214500915298572 ) ) ;
#8470 = CARTESIAN_POINT ( 'NONE',  ( 43.31606138205700063, -10.66749763588699551, 14.47455635838400134 ) ) ;
#8471 = DIRECTION ( 'NONE',  ( 0.000000000000000000, -1.000000000000000000, 0.000000000000000000 ) ) ;
#8472 = CARTESIAN_POINT ( 'NONE',  ( 38.31606138205700063, -22.22127907754186893, 75.30501292736998664 ) ) ;
#8473 = EDGE_LOOP ( 'NONE', ( #3101, #23674, #6838, #17485 ) ) ;
#8474 = ORIENTED_EDGE ( 'NONE', *, *, #1196, .T. ) ;
#8475 = CARTESIAN_POINT ( 'NONE',  ( 33.40064408022072939, 40.76768529863396395, 79.37823623207322044 ) ) ;
#8476 = CARTESIAN_POINT ( 'NONE',  ( 39.02088643472237806, -0.7038408664219175659, 73.73360434286902887 ) ) ;
#8477 = ADVANCED_FACE ( 'NONE', ( #25344 ), #17775, .F. ) ;
#8478 = VECTOR ( 'NONE', #12775, 1000.000000000000227 ) ;
#8479 = EDGE_CURVE ( 'NONE', #16267, #1997, #23425, .T. ) ;
#8480 = CARTESIAN_POINT ( 'NONE',  ( 37.89291511884476904, -21.11368208888610098, 70.26206559358661252 ) ) ;
#8481 = EDGE_LOOP ( 'NONE', ( #1558, #21600, #10008, #25016 ) ) ;
#8482 = ORIENTED_EDGE ( 'NONE', *, *, #16965, .T. ) ;
#8483 = DIRECTION ( 'NONE',  ( -0.000000000000000000, -3.469446951953613400E-15, -1.000000000000000000 ) ) ;
#8484 = CARTESIAN_POINT ( 'NONE',  ( 38.82593461698262871, -8.913682088886101695, 69.62690120949091011 ) ) ;
#8485 = CARTESIAN_POINT ( 'NONE',  ( 39.95015449827720744, -29.00384086642191406, 71.96809898377885872 ) ) ;
#8486 = ADVANCED_FACE ( 'NONE', ( #7468 ), #21756, .T. ) ;
#8487 = EDGE_CURVE ( 'NONE', #14769, #22871, #18154, .T. ) ;
#8488 = ADVANCED_FACE ( 'NONE', ( #22129 ), #16078, .F. ) ;
#8489 = DIRECTION ( 'NONE',  ( 0.000000000000000000, -0.6568589528324746407, 0.7540134720837716742 ) ) ;
#8490 = CARTESIAN_POINT ( 'NONE',  ( 37.50301148336529167, -11.11368208888610276, 69.06206559358666652 ) ) ;
#8491 = DIRECTION ( 'NONE',  ( -1.836970198721029688E-16, -2.999999999999999839E-15, -1.000000000000000000 ) ) ;
#8492 = FACE_OUTER_BOUND ( 'NONE', #15008, .T. ) ;
#8493 = EDGE_CURVE ( 'NONE', #13467, #973, #15568, .T. ) ;
#8494 = ADVANCED_FACE ( 'NONE', ( #23928 ), #15682, .T. ) ;
#8495 = CARTESIAN_POINT ( 'NONE',  ( 43.28398221755340103, 3.843662888489567830, 6.335227539316586665 ) ) ;
#8496 = FACE_BOUND ( 'NONE', #4988, .T. ) ;
#8497 = FACE_OUTER_BOUND ( 'NONE', #3081, .T. ) ;
#8498 = ORIENTED_EDGE ( 'NONE', *, *, #5667, .T. ) ;
#8499 = CARTESIAN_POINT ( 'NONE',  ( 40.26527270485448184, -20.73962474046760818, 75.41239499478379571 ) ) ;
#8500 = EDGE_CURVE ( 'NONE', #10242, #16874, #611, .T. ) ;
#8501 = CARTESIAN_POINT ( 'NONE',  ( 41.81606138205687273, 43.19123852234595518, 61.30501292736988006 ) ) ;
#8502 = VERTEX_POINT ( 'NONE', #14031 ) ;
#8503 = ORIENTED_EDGE ( 'NONE', *, *, #12427, .F. ) ;
#8504 = UNCERTAINTY_MEASURE_WITH_UNIT (LENGTH_MEASURE( 1.000000000000000082E-05 ), #3333, 'distance_accuracy_value', 'NONE');
#8506 = CARTESIAN_POINT ( 'NONE',  ( 36.11133435605973574, -22.00384086642191761, 70.60699637195608602 ) ) ;
#8505 = SHAPE_REPRESENTATION ( 'Upper Tension Leaf Spring', ( #2000 ), #2615 ) ;
#8507 = CARTESIAN_POINT ( 'NONE',  ( 39.38009889167650357, -26.21368208888610951, 72.75271321436730432 ) ) ;
#8508 = CARTESIAN_POINT ( 'NONE',  ( 38.31606138205702194, 1.691238522345987150, 73.11602215082119471 ) ) ;
#8509 = DIRECTION ( 'NONE',  ( -1.734723475976804876E-16, -3.469446951953610245E-15, -1.000000000000000000 ) ) ;
#8510 = DIRECTION ( 'NONE',  ( 0.000000000000000000, -0.6568589528324746407, 0.7540134720837716742 ) ) ;
#8511 = EDGE_LOOP ( 'NONE', ( #2258, #12573, #7715, #5724 ) ) ;
#8512 = CARTESIAN_POINT ( 'NONE',  ( 43.81606138205700063, -27.60498114914042134, 57.04949906928994352 ) ) ;
#8513 = DIRECTION ( 'NONE',  ( 1.000000000000000000, -0.000000000000000000, 0.000000000000000000 ) ) ;
#8514 = CARTESIAN_POINT ( 'NONE',  ( 39.12911128074872380, -1.503840866421912725, 69.06206559358666652 ) ) ;
#8515 = DIRECTION ( 'NONE',  ( -1.000000000000000000, 0.000000000000000000, 0.000000000000000000 ) ) ;
#8516 = DIRECTION ( 'NONE',  ( 0.000000000000000000, 1.000000000000000000, -3.469446951953613400E-15 ) ) ;
#8517 = VECTOR ( 'NONE', #7250, 1000.000000000000000 ) ;
#8518 = CARTESIAN_POINT ( 'NONE',  ( 38.37017380507020192, -8.013682088886108446, 73.11602215082118050 ) ) ;
#8519 = DIRECTION ( 'NONE',  ( 1.000000000000000000, 2.452751524064188892E-15, 1.339444584486322859E-15 ) ) ;
#8520 = CARTESIAN_POINT ( 'NONE',  ( 39.95015449827720744, -20.61368208888610454, 70.79240656858105751 ) ) ;
#8521 = CARTESIAN_POINT ( 'NONE',  ( 32.81606138205700773, 2.887189827768484207, 12.91119156276801228 ) ) ;
#8522 = ADVANCED_FACE ( 'NONE', ( #478 ), #4620, .F. ) ;
#8523 = DIRECTION ( 'NONE',  ( 0.000000000000000000, -0.3299742535180969494, 0.9439899321577399638 ) ) ;
#8524 = CARTESIAN_POINT ( 'NONE',  ( 37.69225076346193504, -23.80384086642191477, 70.42958956619166599 ) ) ;
#8525 = CARTESIAN_POINT ( 'NONE',  ( 38.37017380507020192, -12.01368208888610845, 73.11602215082116629 ) ) ;
#8526 = EDGE_CURVE ( 'NONE', #22825, #11106, #10294, .T. ) ;
#8527 = ORIENTED_EDGE ( 'NONE', *, *, #10047, .T. ) ;
#8528 = CARTESIAN_POINT ( 'NONE',  ( 41.81606138205696510, -1.975699482566714904, -4.057200616784870206 ) ) ;
#8529 = ORIENTED_EDGE ( 'NONE', *, *, #1582, .T. ) ;
#8530 = CIRCLE ( 'NONE', #6464, 2.000000000000000000 ) ;
#8531 = CIRCLE ( 'NONE', #16741, 0.4999999999999943379 ) ;
#8532 = CARTESIAN_POINT ( 'NONE',  ( 38.37017380507018771, -13.60384086642190837, 69.64448340153877837 ) ) ;
#8533 = CARTESIAN_POINT ( 'NONE',  ( 37.31606138205700063, 15.19123852234700500, 71.30501292736995822 ) ) ;
#8534 = CIRCLE ( 'NONE', #11427, 1.000000000000000888 ) ;
#8535 = AXIS2_PLACEMENT_3D ( 'NONE', #15617, #15870, #18073 ) ;
#8536 = CARTESIAN_POINT ( 'NONE',  ( 36.64852494920107517, -3.413682088886104360, 70.89533451361948835 ) ) ;
#8537 = ORIENTED_EDGE ( 'NONE', *, *, #16586, .T. ) ;
#8538 = CARTESIAN_POINT ( 'NONE',  ( 35.86008812008917346, -15.51368208888610667, 71.43714994484034264 ) ) ;
#8539 = ORIENTED_EDGE ( 'NONE', *, *, #11311, .T. ) ;
#8540 = FACE_OUTER_BOUND ( 'NONE', #14110, .T. ) ;
#8541 = DIRECTION ( 'NONE',  ( 0.000000000000000000, 1.000000000000000000, -2.999999999999999839E-15 ) ) ;
#8542 = CARTESIAN_POINT ( 'NONE',  ( 37.89291511884479036, -20.50384086642191406, 72.49843995877330372 ) ) ;
#8543 = ORIENTED_EDGE ( 'NONE', *, *, #10450, .T. ) ;
#8544 = ORIENTED_EDGE ( 'NONE', *, *, #4197, .F. ) ;
#8545 = LINE ( 'NONE', #2596, #19514 ) ;
#8546 = FACE_OUTER_BOUND ( 'NONE', #7262, .T. ) ;
#8547 = CARTESIAN_POINT ( 'NONE',  ( 37.50301148336529877, -22.50384086642191761, 73.69843995877327814 ) ) ;
#8548 = CARTESIAN_POINT ( 'NONE',  ( 44.81606138205700063, -26.74044063519535186, 82.55501292737007191 ) ) ;
#8549 = CARTESIAN_POINT ( 'NONE',  ( 39.75915168707250302, -24.71368208888610241, 70.26145752964249880 ) ) ;
#8550 = CARTESIAN_POINT ( 'NONE',  ( 35.31606138205700773, 8.104266321858618838, 55.82104096753806033 ) ) ;
#8551 = CARTESIAN_POINT ( 'NONE',  ( 36.31606138205701484, -18.45164032183484792, 27.38658776684409091 ) ) ;
#8552 = VECTOR ( 'NONE', #1668, 1000.000000000000000 ) ;
#8553 = ORIENTED_EDGE ( 'NONE', *, *, #15862, .T. ) ;
#8554 = VECTOR ( 'NONE', #13837, 1000.000000000000000 ) ;
#8555 = VECTOR ( 'NONE', #9268, 1000.000000000000000 ) ;
#8556 = PLANE ( 'NONE',  #20307 ) ;
#8557 = LINE ( 'NONE', #6612, #21268 ) ;
#8558 = CARTESIAN_POINT ( 'NONE',  ( 38.26194895904384907, -16.60384086642191548, 73.11602215082116629 ) ) ;
#8559 =( NAMED_UNIT ( * ) SI_UNIT ( $, .STERADIAN. ) SOLID_ANGLE_UNIT ( ) );
#8560 = EDGE_CURVE ( 'NONE', #18636, #2353, #24057, .T. ) ;
#8561 = DIRECTION ( 'NONE',  ( 0.000000000000000000, 0.000000000000000000, 1.000000000000000000 ) ) ;
#8562 = EDGE_CURVE ( 'NONE', #19118, #20855, #10163, .T. ) ;
#8563 = DIRECTION ( 'NONE',  ( -1.000000000000000000, 5.510910596163088391E-31, 1.836970198721029688E-16 ) ) ;
#8564 = DIRECTION ( 'NONE',  ( -1.734723475976814737E-16, 1.000000000000000000, -3.491481338843135327E-15 ) ) ;
#8565 = CARTESIAN_POINT ( 'NONE',  ( 39.29254315202757653, -28.80384086642191832, 72.81632618279320468 ) ) ;
#8566 = CARTESIAN_POINT ( 'NONE',  ( 38.18531088334250967, -5.204193249396280585, 82.80001292736993435 ) ) ;
#8567 = ORIENTED_EDGE ( 'NONE', *, *, #9326, .F. ) ;
#8568 = CARTESIAN_POINT ( 'NONE',  ( 37.25202387243752611, -27.21368208888610241, 70.00779233799262613 ) ) ;
#8569 = ORIENTED_EDGE ( 'NONE', *, *, #4604, .T. ) ;
#8570 = ORIENTED_EDGE ( 'NONE', *, *, #9504, .T. ) ;
#8571 = AXIS2_PLACEMENT_3D ( 'NONE', #4098, #19937, #10277 ) ;
#8572 = CARTESIAN_POINT ( 'NONE',  ( 44.71606138205697789, -5.022037326221690634, -5.474317061061731771 ) ) ;
#8573 = CARTESIAN_POINT ( 'NONE',  ( 43.31606138205700773, -19.13113579875041381, 24.60350147050422720 ) ) ;
#8574 = CARTESIAN_POINT ( 'NONE',  ( 38.63098279924288647, -8.913682088886103472, 70.22690120949091863 ) ) ;
#8575 = VECTOR ( 'NONE', #1845, 1000.000000000000227 ) ;
#8576 = VECTOR ( 'NONE', #22740, 1000.000000000000227 ) ;
#8577 = CARTESIAN_POINT ( 'NONE',  ( 39.51027997493896748, -6.513682088886100452, 71.32335560751961623 ) ) ;
#8578 = VERTEX_POINT ( 'NONE', #22260 ) ;
#8579 = ORIENTED_EDGE ( 'NONE', *, *, #22941, .F. ) ;
#8580 = LINE ( 'NONE', #24263, #2889 ) ;
#8581 = EDGE_CURVE ( 'NONE', #22825, #8063, #10279, .T. ) ;
#8582 = DIRECTION ( 'NONE',  ( 1.000000000000000000, 3.091505625455828697E-15, 4.515976121274772923E-17 ) ) ;
#8583 = ORIENTED_EDGE ( 'NONE', *, *, #5103, .F. ) ;
#8584 = CARTESIAN_POINT ( 'NONE',  ( 39.75915168707251723, -10.90384086642191619, 72.49904802271740323 ) ) ;
#8585 = FACE_OUTER_BOUND ( 'NONE', #1664, .T. ) ;
#8586 = CYLINDRICAL_SURFACE ( 'NONE', #266, 0.2000000000000057288 ) ;
#8587 = ORIENTED_EDGE ( 'NONE', *, *, #20594, .F. ) ;
#8588 = ORIENTED_EDGE ( 'NONE', *, *, #802, .F. ) ;
#8589 = LINE ( 'NONE', #11023, #6309 ) ;
#8590 = CARTESIAN_POINT ( 'NONE',  ( 37.69796330110504101, -5.113682088886100985, 69.66206559358664663 ) ) ;
#8591 = DIRECTION ( 'NONE',  ( 0.000000000000000000, -1.000000000000000000, 2.999999999999999839E-15 ) ) ;
#8592 = DIRECTION ( 'NONE',  ( -3.083952846180990083E-15, -1.000000000000000000, 2.999999999999999839E-15 ) ) ;
#8593 = AXIS2_PLACEMENT_3D ( 'NONE', #9487, #15140, #7169 ) ;
#8594 = CARTESIAN_POINT ( 'NONE',  ( 36.31606138205700063, -1.357181138186128067, 82.80501292736991559 ) ) ;
#8595 = ADVANCED_BREP_SHAPE_REPRESENTATION ( '', ( #17243, #2000 ), #13127 ) ;
#8596 = CARTESIAN_POINT ( 'NONE',  ( 32.31606138205700063, 10.06218483883314718, 67.80501292737497465 ) ) ;
#8597 = LINE ( 'NONE', #16303, #308 ) ;
#8598 = VECTOR ( 'NONE', #230, 1000.000000000000000 ) ;
#8599 = DIRECTION ( 'NONE',  ( 0.000000000000000000, 0.7540134720837676774, 0.6568589528324791926 ) ) ;
#8600 = ORIENTED_EDGE ( 'NONE', *, *, #16178, .T. ) ;
#8601 = VERTEX_POINT ( 'NONE', #2538 ) ;
#8602 = CARTESIAN_POINT ( 'NONE',  ( 40.31606138205700773, 42.19123852234599781, 75.30501292736987295 ) ) ;
#8603 = CARTESIAN_POINT ( 'NONE',  ( 39.73277004305198545, -26.21368208888610951, 73.23812341099225875 ) ) ;
#8604 = STYLED_ITEM ( 'NONE', ( #7019 ), #25265 ) ;
#8605 = CARTESIAN_POINT ( 'NONE',  ( 39.24876120206128860, -24.71368208888610241, 70.63227792289242757 ) ) ;
#8606 = EDGE_LOOP ( 'NONE', ( #24099, #17694, #18517, #12315, #13266, #11306 ) ) ;
#8607 = ORIENTED_EDGE ( 'NONE', *, *, #3854, .T. ) ;
#8608 = EDGE_CURVE ( 'NONE', #20703, #9852, #12115, .T. ) ;
#8609 = DIRECTION ( 'NONE',  ( 0.000000000000000000, 1.000000000000000000, 0.000000000000000000 ) ) ;
#8610 = CARTESIAN_POINT ( 'NONE',  ( 39.82603832034400426, -4.313682088886107380, 72.40698646996135324 ) ) ;
#8611 = CARTESIAN_POINT ( 'NONE',  ( 39.51027997493896748, 0.8961591335780900724, 71.43714994484035685 ) ) ;
#8612 = CARTESIAN_POINT ( 'NONE',  ( 35.64099152588522657, -1.357181138186998925, 80.05501292737000085 ) ) ;
#8613 = CARTESIAN_POINT ( 'NONE',  ( 40.26954217208371034, -8.713682088886100630, 69.89063713639259845 ) ) ;
#8614 = CIRCLE ( 'NONE', #4903, 0.7499999999999985567 ) ;
#8615 = CARTESIAN_POINT ( 'NONE',  ( 43.38751330861478550, 3.099072278388469659, 6.135933108610706732 ) ) ;
#8616 = PLANE ( 'NONE',  #23137 ) ;
#8617 = CARTESIAN_POINT ( 'NONE',  ( 34.06606138205700773, 2.740850673309605412, 6.112030963703427133 ) ) ;
#8618 = CARTESIAN_POINT ( 'NONE',  ( 32.31606138205700063, -21.26162886970023536, 44.16441745890789150 ) ) ;
#8619 = VECTOR ( 'NONE', #9392, 1000.000000000000000 ) ;
#8620 = EDGE_CURVE ( 'NONE', #1727, #11848, #16323, .T. ) ;
#8621 = EDGE_CURVE ( 'NONE', #4551, #19784, #16855, .T. ) ;
#8622 = CARTESIAN_POINT ( 'NONE',  ( 40.11623881305710881, -6.269209199194929027, 82.74378620945387297 ) ) ;
#8623 = ADVANCED_FACE ( 'NONE', ( #20339 ), #6669, .F. ) ;
#8624 = EDGE_CURVE ( 'NONE', #20374, #13086, #12348, .T. ) ;
#8625 = FACE_OUTER_BOUND ( 'NONE', #7528, .T. ) ;
#8626 = EDGE_CURVE ( 'NONE', #15409, #11682, #24684, .T. ) ;
#8627 = AXIS2_PLACEMENT_3D ( 'NONE', #10465, #10720, #18323 ) ;
#8628 = ORIENTED_EDGE ( 'NONE', *, *, #10858, .T. ) ;
#8629 = DIRECTION ( 'NONE',  ( -1.000000000000000000, 0.000000000000000000, 0.000000000000000000 ) ) ;
#8630 = CARTESIAN_POINT ( 'NONE',  ( 33.56606138205700773, 42.19123852234599070, 73.55501292736987295 ) ) ;
#8631 = ORIENTED_EDGE ( 'NONE', *, *, #20401, .T. ) ;
#8632 = ORIENTED_EDGE ( 'NONE', *, *, #1775, .F. ) ;
#8633 = CARTESIAN_POINT ( 'NONE',  ( 36.11133435605973574, -20.00384086642191406, 70.60699637195608602 ) ) ;
#8634 = CIRCLE ( 'NONE', #14800, 0.7500000000000008882 ) ;
#8635 = AXIS2_PLACEMENT_3D ( 'NONE', #14455, #17955, #781 ) ;
#8636 = EDGE_CURVE ( 'NONE', #16929, #18597, #12744, .T. ) ;
#8637 = CARTESIAN_POINT ( 'NONE',  ( 40.33642880535524000, 1.686317911113892620, 72.77780686321129622 ) ) ;
#8638 = DIRECTION ( 'NONE',  ( 0.000000000000000000, -0.7071067811865489050, 0.7071067811865460184 ) ) ;
#8639 = EDGE_CURVE ( 'NONE', #23124, #16518, #3677, .T. ) ;
#8640 = AXIS2_PLACEMENT_3D ( 'NONE', #5735, #13099, #25418 ) ;
#8641 = DIRECTION ( 'NONE',  ( -1.000000000000000000, -1.000000000000000078E-15, 0.000000000000000000 ) ) ;
#8642 = CARTESIAN_POINT ( 'NONE',  ( 33.81606138205700063, 2.191238522347013440, 73.80501292737000085 ) ) ;
#8643 = EDGE_LOOP ( 'NONE', ( #1276, #21965, #6942, #841 ) ) ;
#8644 = CARTESIAN_POINT ( 'NONE',  ( 40.25058685806286007, -6.608132892505640399, 82.70675736217422980 ) ) ;
#8645 = FACE_OUTER_BOUND ( 'NONE', #49, .T. ) ;
#8646 = CARTESIAN_POINT ( 'NONE',  ( 40.33642880535521869, 0.6961591335780878964, 69.98269868914869107 ) ) ;
#8647 = AXIS2_PLACEMENT_3D ( 'NONE', #6074, #11629, #12014 ) ;
#8648 = ORIENTED_EDGE ( 'NONE', *, *, #21347, .F. ) ;
#8649 = LINE ( 'NONE', #23956, #13586 ) ;
#8650 = CIRCLE ( 'NONE', #18102, 1.750000000000001554 ) ;
#8651 = CARTESIAN_POINT ( 'NONE',  ( 43.81608638205700146, 2.761903742731119049, 12.21527246050395377 ) ) ;
#8652 = CARTESIAN_POINT ( 'NONE',  ( 39.95015449827720744, 1.386317911113894130, 70.79240656858108593 ) ) ;
#8653 = DIRECTION ( 'NONE',  ( 1.000000000000000000, 0.000000000000000000, 0.000000000000000000 ) ) ;
#8654 = ADVANCED_FACE ( 'NONE', ( #1113 ), #14534, .T. ) ;
#8655 = CARTESIAN_POINT ( 'NONE',  ( 36.64852494920107517, -21.41368208888610525, 70.89533451361947414 ) ) ;
#8656 = VECTOR ( 'NONE', #19730, 1000.000000000000227 ) ;
#8657 = AXIS2_PLACEMENT_3D ( 'NONE', #14214, #16373, #12285 ) ;
#8658 = DIRECTION ( 'NONE',  ( 1.000000000000000000, -0.000000000000000000, 0.000000000000000000 ) ) ;
#8659 = FACE_OUTER_BOUND ( 'NONE', #6477, .T. ) ;
#8660 = VECTOR ( 'NONE', #25232, 1000.000000000000000 ) ;
#8661 = CARTESIAN_POINT ( 'NONE',  ( 37.38336156205273397, -27.90384086642191264, 70.63227792289245599 ) ) ;
#8662 = CARTESIAN_POINT ( 'NONE',  ( 39.29254315202756231, -14.81368208888610205, 69.94417936956672577 ) ) ;
#8663 = ORIENTED_EDGE ( 'NONE', *, *, #4238, .T. ) ;
#8664 = CARTESIAN_POINT ( 'NONE',  ( 33.31606138205700773, -5.204193249396280585, 82.80501292736992980 ) ) ;
#8665 = ORIENTED_EDGE ( 'NONE', *, *, #21878, .F. ) ;
#8666 = CARTESIAN_POINT ( 'NONE',  ( 36.80608444377001831, -8.303840866421916544, 72.40698646996136745 ) ) ;
#8667 = DIRECTION ( 'NONE',  ( 0.000000000000000000, 1.000000000000000000, -2.999999999999999839E-15 ) ) ;
#8668 = EDGE_CURVE ( 'NONE', #7351, #5806, #2791, .T. ) ;
#8669 = CARTESIAN_POINT ( 'NONE',  ( 38.26194895904383486, -3.013682088886100008, 69.64448340153879258 ) ) ;
#8670 = VERTEX_POINT ( 'NONE', #5135 ) ;
#8671 = CARTESIAN_POINT ( 'NONE',  ( 40.52078840805428683, -16.61368208888610454, 70.60699637195608602 ) ) ;
#8672 = ORIENTED_EDGE ( 'NONE', *, *, #21067, .F. ) ;
#8673 = PLANE ( 'NONE',  #23047 ) ;
#8674 = CARTESIAN_POINT ( 'NONE',  ( 43.31606138205700063, -13.58280000135112964, 20.54174511886706256 ) ) ;
#8675 = CARTESIAN_POINT ( 'NONE',  ( 38.73920764526923932, -11.50384086642191050, 70.26206559358664094 ) ) ;
#8676 = CARTESIAN_POINT ( 'NONE',  ( 40.31606138205701484, -18.45164032183483727, 27.38658776684409091 ) ) ;
#8677 = ORIENTED_EDGE ( 'NONE', *, *, #22941, .T. ) ;
#8678 = DIRECTION ( 'NONE',  ( 1.836970198721029688E-16, 2.999999999999999839E-15, 1.000000000000000000 ) ) ;
#8679 = CARTESIAN_POINT ( 'NONE',  ( 45.81606138205706458, -35.90867894478441968, 74.07034463014319670 ) ) ;
#8680 = CARTESIAN_POINT ( 'NONE',  ( 38.37017380507018771, -19.60384086642191193, 69.04448340153878405 ) ) ;
#8681 = DIRECTION ( 'NONE',  ( -8.673617379884039170E-17, 1.163336342344340343E-15, -1.000000000000000000 ) ) ;
#8682 = CARTESIAN_POINT ( 'NONE',  ( 40.33642880535524000, 1.686317911113892620, 72.77780686321129622 ) ) ;
#8683 = FACE_OUTER_BOUND ( 'NONE', #15037, .T. ) ;
#8684 = EDGE_CURVE ( 'NONE', #21215, #7231, #4744, .T. ) ;
#8685 = LINE ( 'NONE', #16915, #674 ) ;
#8686 = VERTEX_POINT ( 'NONE', #16979 ) ;
#8687 = CARTESIAN_POINT ( 'NONE',  ( 33.66606138205694521, 5.651448314156965580, 4.532640732625139002 ) ) ;
#8688 = DIRECTION ( 'NONE',  ( 1.327674326049709741E-15, -0.4425581086832367506, 0.8967398287344643393 ) ) ;
#8689 = CARTESIAN_POINT ( 'NONE',  ( 36.64852494920107517, -16.20384086642190979, 71.86517103874048473 ) ) ;
#8690 = DIRECTION ( 'NONE',  ( 0.000000000000000000, 0.000000000000000000, 1.000000000000000000 ) ) ;
#8691 = CARTESIAN_POINT ( 'NONE',  ( 31.81606138205700418, 40.39281886181299797, 66.30501292737000085 ) ) ;
#8692 = VERTEX_POINT ( 'NONE', #24432 ) ;
#8693 = AXIS2_PLACEMENT_3D ( 'NONE', #13995, #17991, #5621 ) ;
#8694 = DIRECTION ( 'NONE',  ( 0.000000000000000000, 3.469446951953611033E-15, 1.000000000000000000 ) ) ;
#8695 = VECTOR ( 'NONE', #9119, 1000.000000000000000 ) ;
#8696 = DIRECTION ( 'NONE',  ( 1.000000000000000000, 0.000000000000000000, 0.000000000000000000 ) ) ;
#8697 = CARTESIAN_POINT ( 'NONE',  ( 37.60469502381300799, -2.403840866421910416, 72.26730301774236409 ) ) ;
#8698 = CARTESIAN_POINT ( 'NONE',  ( 37.31005363372398165, -5.457877424396979649, 82.79703358579240557 ) ) ;
#8699 = ORIENTED_EDGE ( 'NONE', *, *, #9409, .F. ) ;
#8700 = CARTESIAN_POINT ( 'NONE',  ( 36.64852494920107517, -25.41368208888610525, 70.89533451361945993 ) ) ;
#8701 = ORIENTED_EDGE ( 'NONE', *, *, #21723, .F. ) ;
#8702 = ORIENTED_EDGE ( 'NONE', *, *, #2002, .T. ) ;
#8703 = CARTESIAN_POINT ( 'NONE',  ( 32.56606138205700773, 45.04446929126255128, 81.37823623207320622 ) ) ;
#8704 = DIRECTION ( 'NONE',  ( 1.734723475976805122E-16, 0.000000000000000000, 1.000000000000000000 ) ) ;
#8705 = CARTESIAN_POINT ( 'NONE',  ( 37.60469502381300799, -28.40384086642191264, 72.26730301774232146 ) ) ;
#8706 = CARTESIAN_POINT ( 'NONE',  ( 38.37017380507018771, -29.60384086642191193, 70.24448340153875847 ) ) ;
#8707 = VERTEX_POINT ( 'NONE', #4867 ) ;
#8708 = VERTEX_POINT ( 'NONE', #20457 ) ;
#8709 = FACE_OUTER_BOUND ( 'NONE', #16050, .T. ) ;
#8710 = FACE_BOUND ( 'NONE', #29, .T. ) ;
#8711 = ORIENTED_EDGE ( 'NONE', *, *, #14606, .T. ) ;
#8712 = CARTESIAN_POINT ( 'NONE',  ( 36.87297107704149823, -11.90384086642190731, 70.26145752964252722 ) ) ;
#8713 = EDGE_CURVE ( 'NONE', #14019, #4191, #8745, .T. ) ;
#8714 = EDGE_CURVE ( 'NONE', #13705, #24513, #12993, .T. ) ;
#8715 = DIRECTION ( 'NONE',  ( -3.965082230804125881E-15, 0.8967398287344645613, 0.4425581086832361399 ) ) ;
#8716 = CYLINDRICAL_SURFACE ( 'NONE', #8107, 1.550000000000002709 ) ;
#8717 = ORIENTED_EDGE ( 'NONE', *, *, #7374, .T. ) ;
#8718 = EDGE_LOOP ( 'NONE', ( #6107, #3604, #11189, #16220, #9507, #14271 ) ) ;
#8719 = MECHANICAL_DESIGN_GEOMETRIC_PRESENTATION_REPRESENTATION (  '', ( #16505 ), #12306 ) ;
#8720 = ORIENTED_EDGE ( 'NONE', *, *, #10957, .T. ) ;
#8721 = CARTESIAN_POINT ( 'NONE',  ( 40.31606138205701484, -18.91453975041205382, 24.37026150481227305 ) ) ;
#8722 = CARTESIAN_POINT ( 'NONE',  ( 36.49096545463212493, -9.513682088886104893, 71.43714994484035685 ) ) ;
#8723 = ORIENTED_EDGE ( 'NONE', *, *, #16871, .T. ) ;
#8724 = LINE ( 'NONE', #24406, #24172 ) ;
#8725 = CARTESIAN_POINT ( 'NONE',  ( 36.31606138205700063, -29.30876147765401640, 69.30501292737010033 ) ) ;
#8726 = DIRECTION ( 'NONE',  ( 1.000000000000000000, 0.000000000000000000, 0.000000000000000000 ) ) ;
#8727 = EDGE_CURVE ( 'NONE', #22626, #20600, #11050, .T. ) ;
#8728 = FACE_OUTER_BOUND ( 'NONE', #1535, .T. ) ;
#8729 = DIRECTION ( 'NONE',  ( -1.000000000000000000, 0.000000000000000000, 0.000000000000000000 ) ) ;
#8730 = LINE ( 'NONE', #20439, #23071 ) ;
#8731 = ORIENTED_EDGE ( 'NONE', *, *, #24497, .F. ) ;
#8732 = ORIENTED_EDGE ( 'NONE', *, *, #4379, .T. ) ;
#8733 = CIRCLE ( 'NONE', #13670, 1.000000000000000888 ) ;
#8734 = DIRECTION ( 'NONE',  ( 0.000000000000000000, 1.000000000000000000, -3.469446951953613400E-15 ) ) ;
#8735 = CARTESIAN_POINT ( 'NONE',  ( 38.26194895904383486, -29.01368208888610312, 69.04448340153878405 ) ) ;
#8736 = CARTESIAN_POINT ( 'NONE',  ( 38.63098279924288647, -18.91368208888609814, 70.22690120949090442 ) ) ;
#8737 = ORIENTED_EDGE ( 'NONE', *, *, #23711, .F. ) ;
#8738 = ORIENTED_EDGE ( 'NONE', *, *, #18084, .F. ) ;
#8739 = AXIS2_PLACEMENT_3D ( 'NONE', #13109, #22499, #16835 ) ;
#8740 = DIRECTION ( 'NONE',  ( 0.000000000000000000, 3.469446951953611033E-15, 1.000000000000000000 ) ) ;
#8741 = CARTESIAN_POINT ( 'NONE',  ( 39.38009889167650357, -0.2136820888861065693, 72.75271321436733274 ) ) ;
#8742 = CARTESIAN_POINT ( 'NONE',  ( 38.93415946300896024, -29.50384086642191050, 69.66206559358660400 ) ) ;
#8743 = DIRECTION ( 'NONE',  ( 1.000000000000000000, 0.000000000000000000, 0.000000000000000000 ) ) ;
#8744 = CARTESIAN_POINT ( 'NONE',  ( 36.36258059203031934, -5.713682088886106847, 72.86986841596736042 ) ) ;
#8745 = LINE ( 'NONE', #10680, #4513 ) ;
#8746 = DIRECTION ( 'NONE',  ( 0.000000000000000000, 1.000000000000000000, -2.999999999999999839E-15 ) ) ;
#8747 = CARTESIAN_POINT ( 'NONE',  ( 45.81606138205700063, -34.55876147765410167, 70.30501292737000085 ) ) ;
#8748 = DIRECTION ( 'NONE',  ( -1.271715504244016160E-15, 0.4425581086832399147, -0.8967398287344627850 ) ) ;
#8749 = CARTESIAN_POINT ( 'NONE',  ( 43.62721312654221606, 3.386191220328446772, 6.178494284004524495 ) ) ;
#8750 = CARTESIAN_POINT ( 'NONE',  ( 40.31606138205700063, 5.691238522346988127, 65.30501292736998664 ) ) ;
#8751 = ADVANCED_FACE ( 'NONE', ( #14906 ), #24812, .F. ) ;
#8752 = CIRCLE ( 'NONE', #15321, 1.550000000000002709 ) ;
#8753 = DIRECTION ( 'NONE',  ( -1.000000000000000000, 0.000000000000000000, 0.000000000000000000 ) ) ;
#8754 = ORIENTED_EDGE ( 'NONE', *, *, #18269, .T. ) ;
#8755 = CARTESIAN_POINT ( 'NONE',  ( 38.44690133353662276, -22.22127907754186893, 75.30501292736998664 ) ) ;
#8756 = VECTOR ( 'NONE', #18403, 1000.000000000000000 ) ;
#8757 = CARTESIAN_POINT ( 'NONE',  ( 42.96606138205697789, -5.898435835062210586, -2.003809078978638247 ) ) ;
#8758 = ORIENTED_EDGE ( 'NONE', *, *, #19689, .F. ) ;
#8759 = VECTOR ( 'NONE', #3178, 1000.000000000000000 ) ;
#8760 = EDGE_LOOP ( 'NONE', ( #1592, #24501, #22780, #23402 ) ) ;
#8761 = UNCERTAINTY_MEASURE_WITH_UNIT (LENGTH_MEASURE( 1.000000000000000082E-05 ), #21579, 'distance_accuracy_value', 'NONE');
#8762 = CARTESIAN_POINT ( 'NONE',  ( 36.11133435605973574, -18.00384086642191050, 70.60699637195608602 ) ) ;
#8763 = CARTESIAN_POINT ( 'NONE',  ( 39.98359781491296161, -22.41368208888610525, 71.86517103874047052 ) ) ;
#8764 = DIRECTION ( 'NONE',  ( 0.000000000000000000, -3.491481338843135327E-15, -1.000000000000000000 ) ) ;
#8765 = AXIS2_PLACEMENT_3D ( 'NONE', #8435, #20021, #8305 ) ;
#8766 = EDGE_CURVE ( 'NONE', #13157, #7024, #12149, .T. ) ;
#8767 = PLANE ( 'NONE',  #11032 ) ;
#8768 = ADVANCED_FACE ( 'NONE', ( #20842 ), #14784, .F. ) ;
#8769 = ORIENTED_EDGE ( 'NONE', *, *, #22897, .F. ) ;
#8770 = LINE ( 'NONE', #2814, #9292 ) ;
#8771 = LINE ( 'NONE', #20742, #17882 ) ;
#8772 = CIRCLE ( 'NONE', #7969, 1.000000000000012657 ) ;
#8773 = CARTESIAN_POINT ( 'NONE',  ( 37.61123632939165873, -27.91368208888610880, 73.73360434286898624 ) ) ;
#8774 = EDGE_LOOP ( 'NONE', ( #14646, #6017, #15771, #1764 ) ) ;
#8775 = ADVANCED_FACE ( 'NONE', ( #3053 ), #10929, .F. ) ;
#8776 = CARTESIAN_POINT ( 'NONE',  ( 34.81606138205687273, 42.19123852234595518, 61.30501292736988006 ) ) ;
#8777 = CARTESIAN_POINT ( 'NONE',  ( 32.81606138205700773, 6.366250835946940967, 6.636353555660927661 ) ) ;
#8778 = CARTESIAN_POINT ( 'NONE',  ( 40.14115730948191185, -2.513682088886103116, 71.32335560751961623 ) ) ;
#8779 = CARTESIAN_POINT ( 'NONE',  ( 32.81606138205700773, -27.25871422114667553, 59.79942265548595515 ) ) ;
#8780 = CIRCLE ( 'NONE', #23152, 1.000000000000000888 ) ;
#8781 = CARTESIAN_POINT ( 'NONE',  ( 37.69796330110504101, -19.11368208888610098, 69.66206559358663242 ) ) ;
#8782 = DIRECTION ( 'NONE',  ( -1.000000000000000000, 0.000000000000000000, 0.000000000000000000 ) ) ;
#8783 = ADVANCED_FACE ( 'NONE', ( #10867 ), #18719, .T. ) ;
#8784 = AXIS2_PLACEMENT_3D ( 'NONE', #6760, #4818, #14613 ) ;
#8785 = CIRCLE ( 'NONE', #21120, 0.2000000000000057288 ) ;
#8786 = CARTESIAN_POINT ( 'NONE',  ( 44.71606138205697079, -4.349482454670842380, -5.142398479549302515 ) ) ;
#8787 = CARTESIAN_POINT ( 'NONE',  ( 39.37952058850012804, -17.00384086642191406, 71.78268878715390144 ) ) ;
#8788 = CARTESIAN_POINT ( 'NONE',  ( 37.80618814713140097, -3.913682088886108801, 73.13360434286904876 ) ) ;
#8789 = ORIENTED_EDGE ( 'NONE', *, *, #3484, .T. ) ;
#8790 = CARTESIAN_POINT ( 'NONE',  ( 33.40064408022072939, 41.67000142393845152, 79.37823623207322044 ) ) ;
#8791 = AXIS2_PLACEMENT_3D ( 'NONE', #4, #4009, #7884 ) ;
#8792 = ORIENTED_EDGE ( 'NONE', *, *, #14135, .T. ) ;
#8793 = CARTESIAN_POINT ( 'NONE',  ( 38.37017380507018771, -3.603840866421907041, 69.64448340153879258 ) ) ;
#8794 = DIRECTION ( 'NONE',  ( -2.048868001712896742E-15, 0.6595716529892345914, -0.7516416929448823669 ) ) ;
#8795 = CARTESIAN_POINT ( 'NONE',  ( 39.75915168707250302, -6.713682088886099741, 70.26145752964252722 ) ) ;
#8796 = VERTEX_POINT ( 'NONE', #24871 ) ;
#8797 = CARTESIAN_POINT ( 'NONE',  ( 39.02088643472237095, -8.913682088886103472, 69.02690120949094421 ) ) ;
#8798 = ORIENTED_EDGE ( 'NONE', *, *, #21655, .T. ) ;
#8799 = FACE_OUTER_BOUND ( 'NONE', #12223, .T. ) ;
#8800 = CARTESIAN_POINT ( 'NONE',  ( 38.00113996487112189, -11.70384086642191335, 70.22690120949091863 ) ) ;
#8801 = EDGE_CURVE ( 'NONE', #19706, #12956, #4931, .T. ) ;
#8802 = DIRECTION ( 'NONE',  ( 1.000000000000000000, 2.490066548941357028E-15, 1.228895056384528999E-15 ) ) ;
#8803 = ADVANCED_FACE ( 'NONE', ( #16914, #18973 ), #1178, .T. ) ;
#8804 = ORIENTED_EDGE ( 'NONE', *, *, #22249, .T. ) ;
#8805 = CARTESIAN_POINT ( 'NONE',  ( 40.64099152588522657, 0.3928188618129990761, 82.55501292736997243 ) ) ;
#8806 = CARTESIAN_POINT ( 'NONE',  ( 42.06606138205700063, 47.04446929126260102, 81.37823623207319201 ) ) ;
#8807 = CARTESIAN_POINT ( 'NONE',  ( 38.37017380507018771, -13.60384086642191193, 69.04448340153878405 ) ) ;
#8808 = AXIS2_PLACEMENT_3D ( 'NONE', #2173, #11739, #23809 ) ;
#8809 = EDGE_CURVE ( 'NONE', #24769, #24795, #16652, .T. ) ;
#8810 = EDGE_CURVE ( 'NONE', #17608, #11322, #22954, .T. ) ;
#8811 = CARTESIAN_POINT ( 'NONE',  ( 36.31606138205700063, -20.32127907754186680, 75.99695190479390305 ) ) ;
#8812 = FILL_AREA_STYLE ('',( #14710 ) ) ;
#8813 = CARTESIAN_POINT ( 'NONE',  ( 37.80618814713140097, -21.91368208888610880, 73.13360434286903455 ) ) ;
#8814 = DIRECTION ( 'NONE',  ( 0.000000000000000000, 1.000000000000000000, 0.000000000000000000 ) ) ;
#8815 = VECTOR ( 'NONE', #9785, 1000.000000000000114 ) ;
#8816 = DIRECTION ( 'NONE',  ( -1.734723475976739795E-16, -4.343580702399009298E-14, -1.000000000000000000 ) ) ;
#8817 = ORIENTED_EDGE ( 'NONE', *, *, #13906, .F. ) ;
#8818 = CARTESIAN_POINT ( 'NONE',  ( 44.06606138205700063, 40.39281886181299797, 82.55501292736983032 ) ) ;
#8819 = DIRECTION ( 'NONE',  ( 0.000000000000000000, 0.000000000000000000, -1.000000000000000000 ) ) ;
#8820 = EDGE_CURVE ( 'NONE', #15268, #18307, #17044, .T. ) ;
#8821 = CARTESIAN_POINT ( 'NONE',  ( 40.14115730948191185, -13.10384086642191015, 71.43714994484031422 ) ) ;
#8822 = CARTESIAN_POINT ( 'NONE',  ( 33.56861364504118228, 3.414468223740023234, 6.349533009087269697 ) ) ;
#8823 = FACE_OUTER_BOUND ( 'NONE', #1397, .T. ) ;
#8824 = VECTOR ( 'NONE', #10740, 1000.000000000000000 ) ;
#8825 = CARTESIAN_POINT ( 'NONE',  ( 45.81606138205694378, 5.290470704224633280, -0.3848988112044732235 ) ) ;
#8826 = CARTESIAN_POINT ( 'NONE',  ( 37.33957961208645315, -23.80384086642191122, 69.94417936956671156 ) ) ;
#8827 = CARTESIAN_POINT ( 'NONE',  ( 36.32862050049384806, -20.56677809167894466, 75.94939806155714734 ) ) ;
#8828 = ORIENTED_EDGE ( 'NONE', *, *, #3875, .T. ) ;
#8829 = EDGE_CURVE ( 'NONE', #14211, #7351, #6377, .T. ) ;
#8830 = AXIS2_PLACEMENT_3D ( 'NONE', #3779, #13712, #11664 ) ;
#8831 = CARTESIAN_POINT ( 'NONE',  ( 39.95015449827720744, -22.61368208888610809, 70.79240656858105751 ) ) ;
#8832 = ORIENTED_EDGE ( 'NONE', *, *, #9974, .T. ) ;
#8833 = ORIENTED_EDGE ( 'NONE', *, *, #9299, .T. ) ;
#8834 = CARTESIAN_POINT ( 'NONE',  ( 42.56606138205700063, -32.75315594507191008, 59.38245422252773409 ) ) ;
#8835 = CARTESIAN_POINT ( 'NONE',  ( 33.31606138205700773, -21.26162886970023536, 44.16441745890789150 ) ) ;
#8836 = CARTESIAN_POINT ( 'NONE',  ( 39.51027997493896748, -2.513682088886099564, 71.32335560751961623 ) ) ;
#8837 = CARTESIAN_POINT ( 'NONE',  ( 37.31647492878122563, 0.6863179111138985045, 70.72433947564853440 ) ) ;
#8838 = VERTEX_POINT ( 'NONE', #15096 ) ;
#8839 = ORIENTED_EDGE ( 'NONE', *, *, #114, .F. ) ;
#8840 = FACE_OUTER_BOUND ( 'NONE', #20088, .T. ) ;
#8841 = LINE ( 'NONE', #5216, #4247 ) ;
#8842 = VERTEX_POINT ( 'NONE', #24483 ) ;
#8843 = CARTESIAN_POINT ( 'NONE',  ( 36.64852494920107517, -4.203840866421910683, 71.86517103874049894 ) ) ;
#8844 = SURFACE_STYLE_FILL_AREA ( #19247 ) ;
#8845 = FACE_OUTER_BOUND ( 'NONE', #10900, .T. ) ;
#8846 = VERTEX_POINT ( 'NONE', #6856 ) ;
#8847 = VECTOR ( 'NONE', #23855, 1000.000000000000227 ) ;
#8848 = VERTEX_POINT ( 'NONE', #5317 ) ;
#8849 = VERTEX_POINT ( 'NONE', #8930 ) ;
#8850 = DIRECTION ( 'NONE',  ( 0.000000000000000000, -0.4425581086832386379, 0.8967398287344635621 ) ) ;
#8851 = CARTESIAN_POINT ( 'NONE',  ( 38.37017380507020192, -4.013682088886107557, 73.11602215082118050 ) ) ;
#8852 = DIRECTION ( 'NONE',  ( 0.000000000000000000, -2.999999999999999839E-15, -1.000000000000000000 ) ) ;
#8853 = CARTESIAN_POINT ( 'NONE',  ( 43.31606138205700063, -13.25716901376041967, 21.21736665487721041 ) ) ;
#8854 = CARTESIAN_POINT ( 'NONE',  ( 35.56606138205702194, -19.40517585842703596, 23.66972737280834238 ) ) ;
#8855 = CARTESIAN_POINT ( 'NONE',  ( 33.31606138205700773, -21.26162886970023536, 44.16441745890789150 ) ) ;
#8856 = ADVANCED_FACE ( 'NONE', ( #13180 ), #10987, .T. ) ;
#8857 = LINE ( 'NONE', #3033, #797 ) ;
#8858 = DIRECTION ( 'NONE',  ( 1.000000000000000000, 0.000000000000000000, 0.000000000000000000 ) ) ;
#8859 = FILL_AREA_STYLE ('',( #13773 ) ) ;
#8860 = EDGE_CURVE ( 'NONE', #6167, #16406, #14712, .T. ) ;
#8861 = PRODUCT_DEFINITION ( 'UNKNOWN', '', #22396, #9016 ) ;
#8862 = PLANE ( 'NONE',  #21856 ) ;
#8863 = VERTEX_POINT ( 'NONE', #24992 ) ;
#8864 = ORIENTED_EDGE ( 'NONE', *, *, #13056, .F. ) ;
#8865 = AXIS2_PLACEMENT_3D ( 'NONE', #3709, #17642, #1640 ) ;
#8866 = CARTESIAN_POINT ( 'NONE',  ( 43.81606138205700063, 2.761903742731119049, 12.21527246050395377 ) ) ;
#8867 = LINE ( 'NONE', #20831, #17679 ) ;
#8868 = CARTESIAN_POINT ( 'NONE',  ( 38.63098279924288647, -14.91368208888609992, 70.22690120949090442 ) ) ;
#8869 = VERTEX_POINT ( 'NONE', #16774 ) ;
#8870 = ORIENTED_EDGE ( 'NONE', *, *, #18953, .F. ) ;
#8871 = DIRECTION ( 'NONE',  ( -1.000000000000000000, 0.000000000000000000, 0.000000000000000000 ) ) ;
#8872 = CARTESIAN_POINT ( 'NONE',  ( 37.33957961208646736, 0.1863179111138910105, 72.81632618279323310 ) ) ;
#8873 = CARTESIAN_POINT ( 'NONE',  ( 38.26194895904384907, -26.60384086642191548, 73.11602215082115208 ) ) ;
#8874 = DIRECTION ( 'NONE',  ( -1.327674326049719602E-15, 0.4425581086832399147, -0.8967398287344627850 ) ) ;
#8875 = ADVANCED_FACE ( 'NONE', ( #22574, #24743, #7379, #24610 ), #18838, .T. ) ;
#8876 = CARTESIAN_POINT ( 'NONE',  ( 40.52078840805428683, -10.61368208888610631, 70.60699637195608602 ) ) ;
#8877 = DIRECTION ( 'NONE',  ( 0.000000000000000000, -2.999999999999999839E-15, -1.000000000000000000 ) ) ;
#8878 = CARTESIAN_POINT ( 'NONE',  ( 33.31606138205700773, -12.97731741051368459, 21.08248588348817876 ) ) ;
#8879 = PLANE ( 'NONE',  #19226 ) ;
#8880 = VECTOR ( 'NONE', #9405, 1000.000000000000000 ) ;
#8881 = DIRECTION ( 'NONE',  ( 1.734723475976804876E-16, 3.552713678800500140E-15, 1.000000000000000000 ) ) ;
#8882 = CARTESIAN_POINT ( 'NONE',  ( 39.64148445914975127, -5.676854949425127472, 82.78922245135619562 ) ) ;
#8883 = DIRECTION ( 'NONE',  ( -1.000000000000000000, -1.734723475976804876E-16, 1.734723475976814737E-16 ) ) ;
#8884 = DIRECTION ( 'NONE',  ( -1.000000000000000000, -6.938893903907222067E-15, 0.000000000000000000 ) ) ;
#8885 = EDGE_CURVE ( 'NONE', #2290, #7039, #3165, .T. ) ;
#8886 = ORIENTED_EDGE ( 'NONE', *, *, #5242, .F. ) ;
#8887 = CARTESIAN_POINT ( 'NONE',  ( 43.31606138205700063, -5.204193249396277032, 83.30501292736992980 ) ) ;
#8888 = DIRECTION ( 'NONE',  ( -2.442401846778130416E-15, 0.8967398287344627850, 0.4425581086832399147 ) ) ;
#8889 = ORIENTED_EDGE ( 'NONE', *, *, #18613, .F. ) ;
#8890 = VERTEX_POINT ( 'NONE', #14842 ) ;
#8891 = CARTESIAN_POINT ( 'NONE',  ( 36.07789103942399578, -14.20384086642191512, 72.05058123536544201 ) ) ;
#8892 = CARTESIAN_POINT ( 'NONE',  ( 39.29254315202756231, -20.81368208888610027, 69.94417936956672577 ) ) ;
#8893 = CARTESIAN_POINT ( 'NONE',  ( 44.31606138205700063, -20.55619265724211076, 44.11584019928223910 ) ) ;
#8894 = CARTESIAN_POINT ( 'NONE',  ( 46.81606138205695089, 5.290470704224636833, -0.3848988112044732235 ) ) ;
#8895 =( NAMED_UNIT ( * ) SI_UNIT ( $, .STERADIAN. ) SOLID_ANGLE_UNIT ( ) );
#8896 = ORIENTED_EDGE ( 'NONE', *, *, #22996, .T. ) ;
#8897 = CARTESIAN_POINT ( 'NONE',  ( 44.81606138205700063, -24.55876147765400574, 72.80501292737008612 ) ) ;
#8898 = DIRECTION ( 'NONE',  ( -2.452751524064188892E-15, 1.000000000000000000, 0.000000000000000000 ) ) ;
#8899 = ADVANCED_FACE ( 'NONE', ( #12928 ), #921, .F. ) ;
#8900 = CARTESIAN_POINT ( 'NONE',  ( 39.64521430340305841, 1.196159133578081457, 73.30173637941821596 ) ) ;
#8901 = EDGE_LOOP ( 'NONE', ( #22692, #17125, #10732, #15030 ) ) ;
#8902 = FILL_AREA_STYLE_COLOUR ( '', #2411 ) ;
#8903 = CARTESIAN_POINT ( 'NONE',  ( 28.81606138205698997, -6.548589660139430002, -8.069948661059614281 ) ) ;
#8904 = CARTESIAN_POINT ( 'NONE',  ( 37.80618814713140097, -1.913682088886106136, 73.13360434286904876 ) ) ;
#8905 = DIRECTION ( 'NONE',  ( -1.000000000000000000, -7.979170143241514824E-17, 1.148292460158762122E-16 ) ) ;
#8906 = ORIENTED_EDGE ( 'NONE', *, *, #17941, .T. ) ;
#8907 = CARTESIAN_POINT ( 'NONE',  ( 39.98359781491296161, -20.41368208888610525, 71.86517103874047052 ) ) ;
#8908 = CARTESIAN_POINT ( 'NONE',  ( 39.53940869104339839, -21.82950711158638768, 75.81284195793978142 ) ) ;
#8909 = PLANE ( 'NONE',  #7982 ) ;
#8910 = CARTESIAN_POINT ( 'NONE',  ( 37.69225076346193504, -21.80384086642191122, 70.42958956619168021 ) ) ;
#8911 = CARTESIAN_POINT ( 'NONE',  ( 39.38009889167650357, -4.213682088886106847, 72.75271321436733274 ) ) ;
#8912 = DIRECTION ( 'NONE',  ( -0.000000000000000000, 1.000000000000000000, -3.225463739888140187E-15 ) ) ;
#8913 = ORIENTED_EDGE ( 'NONE', *, *, #1092, .F. ) ;
#8914 = CARTESIAN_POINT ( 'NONE',  ( 38.82593461698265003, -2.703840866421916012, 73.13360434286904876 ) ) ;
#8915 = CARTESIAN_POINT ( 'NONE',  ( 44.06606138205700063, 40.39281886181299797, 82.55501292736983032 ) ) ;
#8916 = CARTESIAN_POINT ( 'NONE',  ( 36.68196826583682935, -5.613682088886105426, 71.96809898377890136 ) ) ;
#8917 = ORIENTED_EDGE ( 'NONE', *, *, #17637, .F. ) ;
#8918 = CARTESIAN_POINT ( 'NONE',  ( 36.29569395875879678, -7.313682088886101162, 69.98269868914869107 ) ) ;
#8919 = ORIENTED_EDGE ( 'NONE', *, *, #7554, .F. ) ;
#8920 = FACE_OUTER_BOUND ( 'NONE', #11179, .T. ) ;
#8921 = CARTESIAN_POINT ( 'NONE',  ( 37.12184278917507640, -10.10384086642191193, 71.32335560751961623 ) ) ;
#8922 = ORIENTED_EDGE ( 'NONE', *, *, #23181, .F. ) ;
#8923 = ORIENTED_EDGE ( 'NONE', *, *, #24642, .T. ) ;
#8924 = CARTESIAN_POINT ( 'NONE',  ( 38.31606138205700063, 38.69123852234598360, 71.30501292737018559 ) ) ;
#8925 = PLANE ( 'NONE',  #3830 ) ;
#8926 = ADVANCED_FACE ( 'NONE', ( #5193 ), #13051, .F. ) ;
#8927 = CARTESIAN_POINT ( 'NONE',  ( 37.50301148336529877, -14.50384086642191761, 73.69843995877327814 ) ) ;
#8928 = CARTESIAN_POINT ( 'NONE',  ( 36.99021717747880444, -21.74921351108408984, 75.81633765512088985 ) ) ;
#8929 = CARTESIAN_POINT ( 'NONE',  ( 38.82593461698262871, -22.91368208888609459, 69.62690120949091011 ) ) ;
#8930 = CARTESIAN_POINT ( 'NONE',  ( 36.31606138205700063, 42.19123852234596939, 65.30501292736988717 ) ) ;
#8931 = CARTESIAN_POINT ( 'NONE',  ( 43.31606138205700063, -12.40281258615395465, 20.95421293576468358 ) ) ;
#8932 = EDGE_LOOP ( 'NONE', ( #15408, #19778 ) ) ;
#8933 = LINE ( 'NONE', #5066, #5921 ) ;
#8934 = FACE_OUTER_BOUND ( 'NONE', #11469, .T. ) ;
#8935 = CARTESIAN_POINT ( 'NONE',  ( 36.68196826583682935, -18.00384086642191406, 70.79240656858107172 ) ) ;
#8936 = TOROIDAL_SURFACE ( 'NONE', #23312, 1.250000000000000000, 0.5000000000000000000 ) ;
#8937 = CARTESIAN_POINT ( 'NONE',  ( 44.81606138205700063, -26.74044063519535186, 82.50501292737007475 ) ) ;
#8938 = EDGE_CURVE ( 'NONE', #868, #1958, #8530, .T. ) ;
#8939 = CARTESIAN_POINT ( 'NONE',  ( 37.69796330110504101, -23.11368208888609743, 69.66206559358660400 ) ) ;
#8940 = AXIS2_PLACEMENT_3D ( 'NONE', #11254, #19106, #1442 ) ;
#8941 = AXIS2_PLACEMENT_3D ( 'NONE', #14106, #4324, #16150 ) ;
#8942 = ADVANCED_FACE ( 'NONE', ( #13553, #8 ), #7889, .T. ) ;
#8943 = LINE ( 'NONE', #14353, #25032 ) ;
#8944 = ADVANCED_FACE ( 'NONE', ( #15737 ), #15859, .T. ) ;
#8945 = CARTESIAN_POINT ( 'NONE',  ( 39.29254315202757653, -22.80384086642191477, 72.81632618279321889 ) ) ;
#8946 = EDGE_CURVE ( 'NONE', #7685, #9479, #17551, .T. ) ;
#8947 = DIRECTION ( 'NONE',  ( -1.000000000000000000, 0.000000000000000000, 0.000000000000000000 ) ) ;
#8948 = CARTESIAN_POINT ( 'NONE',  ( 37.33957961208646736, -23.81368208888611093, 72.81632618279320468 ) ) ;
#8949 = ORIENTED_EDGE ( 'NONE', *, *, #10543, .F. ) ;
#8950 = ORIENTED_EDGE ( 'NONE', *, *, #758, .T. ) ;
#8951 = CARTESIAN_POINT ( 'NONE',  ( 33.56477571746443544, 3.418883076854447367, 6.349191931652266696 ) ) ;
#8952 = CARTESIAN_POINT ( 'NONE',  ( 45.81606138205700063, 46.92314894770293421, 79.37823623207319201 ) ) ;
#8953 = CARTESIAN_POINT ( 'NONE',  ( 37.12184278917507640, -1.513682088886101784, 71.43714994484035685 ) ) ;
#8954 = CARTESIAN_POINT ( 'NONE',  ( 37.69225076346193504, 0.1863179111138979493, 72.33091598616827866 ) ) ;
#8955 = ORIENTED_EDGE ( 'NONE', *, *, #4067, .T. ) ;
#8956 = ORIENTED_EDGE ( 'NONE', *, *, #3932, .F. ) ;
#8957 = DIRECTION ( 'NONE',  ( 2.792262043613788535E-15, -0.8967398287344627850, -0.4425581086832399147 ) ) ;
#8958 = DIRECTION ( 'NONE',  ( 0.000000000000000000, 0.1918498038142811835, -0.9814242980364923374 ) ) ;
#8959 = ORIENTED_EDGE ( 'NONE', *, *, #15223, .F. ) ;
#8960 = EDGE_CURVE ( 'NONE', #7089, #16232, #23588, .T. ) ;
#8961 = DIRECTION ( 'NONE',  ( 1.000000000000000000, 1.734723475976804876E-16, -1.734723475976814737E-16 ) ) ;
#8962 = CARTESIAN_POINT ( 'NONE',  ( 37.25202387243754032, -4.403840866421916189, 72.75271321436733274 ) ) ;
#8963 = VECTOR ( 'NONE', #11754, 1000.000000000000000 ) ;
#8964 = EDGE_CURVE ( 'NONE', #8502, #2101, #1923, .T. ) ;
#8965 = AXIS2_PLACEMENT_3D ( 'NONE', #5957, #13312, #17424 ) ;
#8966 = CARTESIAN_POINT ( 'NONE',  ( 34.66606138205693810, 6.105630034208187062, 5.871938670042847974 ) ) ;
#8967 = CYLINDRICAL_SURFACE ( 'NONE', #5673, 0.4999999999999998890 ) ;
#8968 = VERTEX_POINT ( 'NONE', #7759 ) ;
#8969 = VERTEX_POINT ( 'NONE', #5569 ) ;
#8970 = EDGE_LOOP ( 'NONE', ( #7111, #17634, #22349, #9503 ) ) ;
#8971 = CARTESIAN_POINT ( 'NONE',  ( 31.01606138205700347, 44.92314894770294131, 81.37823623207322044 ) ) ;
#8972 = CARTESIAN_POINT ( 'NONE',  ( 38.37017380507020192, -0.01368208888610777940, 73.11602215082118050 ) ) ;
#8973 = EDGE_CURVE ( 'NONE', #13994, #2738, #15103, .T. ) ;
#8974 = ORIENTED_EDGE ( 'NONE', *, *, #446, .T. ) ;
#8975 = CYLINDRICAL_SURFACE ( 'NONE', #20077, 4.000000000000003553 ) ;
#8976 = LINE ( 'NONE', #1353, #14511 ) ;
#8977 = ORIENTED_EDGE ( 'NONE', *, *, #4369, .F. ) ;
#8978 = DIRECTION ( 'NONE',  ( 0.000000000000000000, 1.000000000000000000, -2.643388153869420409E-15 ) ) ;
#8979 = LINE ( 'NONE', #22620, #7576 ) ;
#8980 = AXIS2_PLACEMENT_3D ( 'NONE', #22277, #20739, #3074 ) ;
#8981 = DIRECTION ( 'NONE',  ( -1.000000000000000000, 0.000000000000000000, 0.000000000000000000 ) ) ;
#8982 = DIRECTION ( 'NONE',  ( -1.000000000000000000, -1.000000000000000078E-15, 0.000000000000000000 ) ) ;
#8983 = AXIS2_PLACEMENT_3D ( 'NONE', #12045, #4310, #18213 ) ;
#8984 = VECTOR ( 'NONE', #1352, 1000.000000000000000 ) ;
#8985 = DIRECTION ( 'NONE',  ( 0.000000000000000000, -2.999999999999999839E-15, -1.000000000000000000 ) ) ;
#8986 = VERTEX_POINT ( 'NONE', #17808 ) ;
#8987 = ORIENTED_EDGE ( 'NONE', *, *, #13879, .F. ) ;
#8988 = LINE ( 'NONE', #11176, #21072 ) ;
#8989 = DIRECTION ( 'NONE',  ( -1.734723475976804876E-16, 1.000000000000000000, 3.009265538105065326E-32 ) ) ;
#8990 = CARTESIAN_POINT ( 'NONE',  ( 37.89291511884476904, -19.11368208888609388, 70.26206559358661252 ) ) ;
#8991 = ORIENTED_EDGE ( 'NONE', *, *, #24059, .T. ) ;
#8992 = ORIENTED_EDGE ( 'NONE', *, *, #14928, .T. ) ;
#8993 = DIRECTION ( 'NONE',  ( -1.000000000000000000, 5.510910596163088391E-31, 1.836970198721029688E-16 ) ) ;
#8994 = CARTESIAN_POINT ( 'NONE',  ( 40.14115730948191185, -0.5136820888861047818, 71.32335560751961623 ) ) ;
#8995 = CARTESIAN_POINT ( 'NONE',  ( 39.98359781491296161, -23.20384086642191335, 70.89533451361945993 ) ) ;
#8996 = DIRECTION ( 'NONE',  ( 0.000000000000000000, -0.5706330172266919076, 0.8212051873014208914 ) ) ;
#8997 = CARTESIAN_POINT ( 'NONE',  ( 36.11133435605973574, -9.613682088886104538, 72.15350918040385864 ) ) ;
#8998 = DIRECTION ( 'NONE',  ( 1.000000000000000000, 2.602085213965208275E-15, 0.000000000000000000 ) ) ;
#8999 = ORIENTED_EDGE ( 'NONE', *, *, #6072, .F. ) ;
#9000 = VECTOR ( 'NONE', #21230, 1000.000000000000000 ) ;
#9001 = DIRECTION ( 'NONE',  ( 0.000000000000000000, -3.965082230804126670E-15, -1.000000000000000000 ) ) ;
#9002 = EDGE_CURVE ( 'NONE', #9093, #6757, #6077, .T. ) ;
#9003 = EDGE_CURVE ( 'NONE', #23360, #5934, #17910, .T. ) ;
#9004 = DIRECTION ( 'NONE',  ( 0.000000000000000000, -4.343580702399009298E-14, -1.000000000000000000 ) ) ;
#9005 = VECTOR ( 'NONE', #11855, 1000.000000000000000 ) ;
#9006 = CARTESIAN_POINT ( 'NONE',  ( 32.81606138205700773, -34.55876147765707174, 70.30501292736873609 ) ) ;
#9007 = CARTESIAN_POINT ( 'NONE',  ( 40.56606138205700773, 5.719301844480432884, 2.701924129460374413 ) ) ;
#9008 = CARTESIAN_POINT ( 'NONE',  ( 33.31606138205700773, -16.77230293220685198, 77.52306850662458260 ) ) ;
#9009 = VECTOR ( 'NONE', #18306, 1000.000000000000000 ) ;
#9010 = CARTESIAN_POINT ( 'NONE',  ( 42.96606138205698500, -7.345467396808729177, -0.7664329602057526891 ) ) ;
#9011 = ORIENTED_EDGE ( 'NONE', *, *, #12683, .F. ) ;
#9012 = DIRECTION ( 'NONE',  ( 1.000000000000000000, 0.000000000000000000, 0.000000000000000000 ) ) ;
#9013 = CARTESIAN_POINT ( 'NONE',  ( 43.81606138205700063, 41.44123852234599070, 73.55501292736987295 ) ) ;
#9014 = ORIENTED_EDGE ( 'NONE', *, *, #1300, .F. ) ;
#9015 = ORIENTED_EDGE ( 'NONE', *, *, #8159, .T. ) ;
#9016 = PRODUCT_DEFINITION_CONTEXT ( 'detailed design', #23629, 'design' ) ;
#9017 = PRESENTATION_LAYER_ASSIGNMENT (  '', '', ( #15978 ) ) ;
#9018 = CARTESIAN_POINT ( 'NONE',  ( 37.50301148336529877, -16.50384086642191761, 73.69843995877327814 ) ) ;
#9019 = VECTOR ( 'NONE', #13724, 1000.000000000000000 ) ;
#9020 = CARTESIAN_POINT ( 'NONE',  ( 37.25202387243752611, -23.21368208888610241, 70.00779233799262613 ) ) ;
#9021 = LINE ( 'NONE', #10818, #18964 ) ;
#9022 = CIRCLE ( 'NONE', #21755, 2.000000000000000000 ) ;
#9023 = DIRECTION ( 'NONE',  ( 0.000000000000000000, -0.8212051873014252212, -0.5706330172266858014 ) ) ;
#9024 = FILL_AREA_STYLE ('',( #15054 ) ) ;
#9025 = ORIENTED_EDGE ( 'NONE', *, *, #24235, .F. ) ;
#9026 = CARTESIAN_POINT ( 'NONE',  ( 36.81465384343994884, 41.43850569188389699, 79.37823623207322044 ) ) ;
#9027 = DIRECTION ( 'NONE',  ( 1.000000000000000000, 2.452751524064188892E-15, 1.339444584486322859E-15 ) ) ;
#9028 = CARTESIAN_POINT ( 'NONE',  ( 39.02088643472237095, -26.91368208888610170, 69.02690120949091579 ) ) ;
#9029 = ORIENTED_EDGE ( 'NONE', *, *, #16831, .T. ) ;
#9030 = ADVANCED_FACE ( 'NONE', ( #7499 ), #21278, .F. ) ;
#9031 = VECTOR ( 'NONE', #20083, 1000.000000000000000 ) ;
#9032 = DIRECTION ( 'NONE',  ( 1.000000000000000000, 2.999999999999999839E-15, -5.603103565922885572E-33 ) ) ;
#9034 = ADVANCED_FACE ( 'NONE', ( #2069 ), #13415, .T. ) ;
#9033 = CARTESIAN_POINT ( 'NONE',  ( 34.81606138205696510, -1.975699482566735776, -4.057200616784870206 ) ) ;
#9035 = CARTESIAN_POINT ( 'NONE',  ( 37.69796330110504101, -3.113682088886098764, 69.66206559358663242 ) ) ;
#9036 = FACE_OUTER_BOUND ( 'NONE', #21597, .T. ) ;
#9037 = ADVANCED_FACE ( 'NONE', ( #19217 ), #8020, .F. ) ;
#9038 = CARTESIAN_POINT ( 'NONE',  ( 40.14115730948191185, -22.51368208888610312, 71.32335560751960202 ) ) ;
#9039 = VECTOR ( 'NONE', #23550, 1000.000000000000000 ) ;
#9040 = VECTOR ( 'NONE', #2829, 1000.000000000000227 ) ;
#9041 = DIRECTION ( 'NONE',  ( 0.000000000000000000, -0.4425581086832404143, 0.8967398287344625629 ) ) ;
#9042 = DIRECTION ( 'NONE',  ( 1.734723475976804876E-16, 3.469446951953610245E-15, 1.000000000000000000 ) ) ;
#9043 = CIRCLE ( 'NONE', #14364, 0.5000000000000004441 ) ;
#9044 = CARTESIAN_POINT ( 'NONE',  ( 39.51027997493896748, -17.10384086642191193, 71.43714994484032843 ) ) ;
#9045 = CARTESIAN_POINT ( 'NONE',  ( 36.49096545463212493, -7.513682088886102228, 71.43714994484035685 ) ) ;
#9046 = ORIENTED_EDGE ( 'NONE', *, *, #13974, .T. ) ;
#9047 = DIRECTION ( 'NONE',  ( 1.000000000000000000, 0.000000000000000000, 0.000000000000000000 ) ) ;
#9048 = ADVANCED_FACE ( 'NONE', ( #15351 ), #23323, .F. ) ;
#9049 = ORIENTED_EDGE ( 'NONE', *, *, #16308, .F. ) ;
#9050 = AXIS2_PLACEMENT_3D ( 'NONE', #709, #1232, #18760 ) ;
#9051 = CARTESIAN_POINT ( 'NONE',  ( 39.75915168707251723, -6.903840866421915301, 72.49904802271740323 ) ) ;
#9052 = FACE_OUTER_BOUND ( 'NONE', #5018, .T. ) ;
#9053 = VECTOR ( 'NONE', #12365, 1000.000000000000114 ) ;
#9054 = CARTESIAN_POINT ( 'NONE',  ( 36.49096545463212493, -5.513682088886105781, 71.43714994484035685 ) ) ;
#9055 = EDGE_LOOP ( 'NONE', ( #15941, #7355 ) ) ;
#9056 = CARTESIAN_POINT ( 'NONE',  ( 38.26194895904383486, -9.013682088886101340, 69.04448340153881247 ) ) ;
#9057 = ORIENTED_EDGE ( 'NONE', *, *, #9541, .F. ) ;
#9058 = PLANE ( 'NONE',  #23853 ) ;
#9059 = CARTESIAN_POINT ( 'NONE',  ( 37.25260217561390874, -10.00384086642191406, 70.97781676520604321 ) ) ;
#9060 = CIRCLE ( 'NONE', #9460, 1.549999999999995826 ) ;
#9061 = DIRECTION ( 'NONE',  ( 1.000000000000000000, 0.000000000000000000, -0.000000000000000000 ) ) ;
#9062 = VERTEX_POINT ( 'NONE', #14438 ) ;
#9063 = CARTESIAN_POINT ( 'NONE',  ( 36.31606138205700773, -20.71832067026706525, 29.15499406670137006 ) ) ;
#9064 = DIRECTION ( 'NONE',  ( -1.000000000000000000, 0.000000000000000000, 0.000000000000000000 ) ) ;
#9065 = CARTESIAN_POINT ( 'NONE',  ( 36.98690846071097127, -17.80384086642191122, 69.45876917294175712 ) ) ;
#9066 = VECTOR ( 'NONE', #24672, 1000.000000000000000 ) ;
#9067 = CARTESIAN_POINT ( 'NONE',  ( 36.72121174906109786, -21.47450125013314803, 75.83383770706140581 ) ) ;
#9068 = FACE_OUTER_BOUND ( 'NONE', #17879, .T. ) ;
#9069 = CARTESIAN_POINT ( 'NONE',  ( 38.37017380507020192, -22.01368208888611022, 73.11602215082116629 ) ) ;
#9070 = CARTESIAN_POINT ( 'NONE',  ( 31.81606138205700418, 41.44123852234599781, 75.30501292736988717 ) ) ;
#9071 = DIRECTION ( 'NONE',  ( 1.000000000000000000, 0.000000000000000000, 0.000000000000000000 ) ) ;
#9072 = CIRCLE ( 'NONE', #12364, 1.000000000000000000 ) ;
#9073 = ORIENTED_EDGE ( 'NONE', *, *, #7129, .F. ) ;
#9074 = DIRECTION ( 'NONE',  ( 0.000000000000000000, -1.000000000000000000, 3.469446951953611033E-15 ) ) ;
#9075 = CYLINDRICAL_SURFACE ( 'NONE', #21288, 1.249999999999998890 ) ;
#9076 = CARTESIAN_POINT ( 'NONE',  ( 39.82603832034401137, -9.303840866421907663, 70.35351908239860563 ) ) ;
#9077 = APPLICATION_PROTOCOL_DEFINITION ( 'draft international standard', 'automotive_design', 1998, #24918 ) ;
#9078 = CYLINDRICAL_SURFACE ( 'NONE', #25208, 0.2000000000000057288 ) ;
#9079 = CARTESIAN_POINT ( 'NONE',  ( 39.82603832034400426, -22.31368208888610738, 72.40698646996133903 ) ) ;
#9080 = FACE_OUTER_BOUND ( 'NONE', #5748, .T. ) ;
#9081 = EDGE_CURVE ( 'NONE', #11508, #20175, #15976, .T. ) ;
#9082 = CARTESIAN_POINT ( 'NONE',  ( 36.64852494920107517, -22.20384086642191335, 71.86517103874048473 ) ) ;
#9083 = DIRECTION ( 'NONE',  ( -1.000000000000000000, -3.091505625455828697E-15, -4.515976121274772923E-17 ) ) ;
#9084 = AXIS2_PLACEMENT_3D ( 'NONE', #13418, #9691, #1430 ) ;
#9085 = CARTESIAN_POINT ( 'NONE',  ( 39.98359781491296161, -24.41368208888610525, 71.86517103874045631 ) ) ;
#9086 = ORIENTED_EDGE ( 'NONE', *, *, #20456, .F. ) ;
#9087 = VERTEX_POINT ( 'NONE', #6575 ) ;
#9088 = CARTESIAN_POINT ( 'NONE',  ( 31.81606138205700418, 41.44123852234599070, 73.55501292736987295 ) ) ;
#9089 = DIRECTION ( 'NONE',  ( -1.000000000000000000, 6.018531076210103283E-31, 1.734723475976805122E-16 ) ) ;
#9090 = AXIS2_PLACEMENT_3D ( 'NONE', #15553, #19417, #25330 ) ;
#9091 = CARTESIAN_POINT ( 'NONE',  ( 37.25260217561390874, -1.613682088886101651, 71.78268878715394408 ) ) ;
#9092 = VERTEX_POINT ( 'NONE', #4649 ) ;
#9093 = VERTEX_POINT ( 'NONE', #4276 ) ;
#9094 = CARTESIAN_POINT ( 'NONE',  ( 43.23147868389327897, 40.76768529863396395, 79.57823623207323749 ) ) ;
#9095 = CARTESIAN_POINT ( 'NONE',  ( 43.29192581567074427, 3.843594479409538689, 6.333537542383846031 ) ) ;
#9096 = FILL_AREA_STYLE_COLOUR ( '', #2106 ) ;
#9097 = CARTESIAN_POINT ( 'NONE',  ( 38.37017380507018771, -1.603840866421908595, 69.64448340153879258 ) ) ;
#9098 = EDGE_CURVE ( 'NONE', #24470, #2345, #4527, .T. ) ;
#9099 = CARTESIAN_POINT ( 'NONE',  ( 40.10895460087045450, 8.484131741160446438, 65.30501292736998664 ) ) ;
#9100 = EDGE_CURVE ( 'NONE', #194, #18550, #20366, .T. ) ;
#9101 = LINE ( 'NONE', #16942, #17996 ) ;
#9102 = ADVANCED_FACE ( 'NONE', ( #18433 ), #18315, .F. ) ;
#9103 = ORIENTED_EDGE ( 'NONE', *, *, #14752, .T. ) ;
#9104 = VERTEX_POINT ( 'NONE', #10197 ) ;
#9105 = ADVANCED_FACE ( 'NONE', ( #763 ), #16355, .F. ) ;
#9106 = ORIENTED_EDGE ( 'NONE', *, *, #18939, .F. ) ;
#9107 = DIRECTION ( 'NONE',  ( -1.000000000000000000, 1.115179377413661005E-30, 3.717264591378870232E-16 ) ) ;
#9108 = VECTOR ( 'NONE', #6633, 1000.000000000000000 ) ;
#9109 = CARTESIAN_POINT ( 'NONE',  ( 37.69796330110504101, -1.113682088886101207, 69.66206559358664663 ) ) ;
#9110 = CARTESIAN_POINT ( 'NONE',  ( 37.25202387243754032, -28.40384086642191619, 72.75271321436730432 ) ) ;
#9111 = DIRECTION ( 'NONE',  ( 1.000000000000000000, 2.602085213965208275E-15, 0.000000000000000000 ) ) ;
#9112 = VECTOR ( 'NONE', #8441, 1000.000000000000000 ) ;
#9113 = ORIENTED_EDGE ( 'NONE', *, *, #18713, .T. ) ;
#9114 = CARTESIAN_POINT ( 'NONE',  ( 43.31606138205700773, -19.92642959707777806, 24.72592537066031682 ) ) ;
#9115 = ADVANCED_FACE ( 'NONE', ( #2571 ), #22161, .T. ) ;
#9116 = CARTESIAN_POINT ( 'NONE',  ( 40.64099152588522657, 1.142818861812999742, 83.30501292736997243 ) ) ;
#9117 = FACE_BOUND ( 'NONE', #14245, .T. ) ;
#9118 = FACE_OUTER_BOUND ( 'NONE', #18925, .T. ) ;
#9119 = DIRECTION ( 'NONE',  ( -6.505213034913089466E-17, 1.000000000000000000, -3.491481338843135327E-15 ) ) ;
#9120 = ORIENTED_EDGE ( 'NONE', *, *, #10668, .F. ) ;
#9121 = ORIENTED_EDGE ( 'NONE', *, *, #12563, .F. ) ;
#9122 = DIRECTION ( 'NONE',  ( 0.000000000000000000, -0.5706330172266930179, 0.8212051873014202252 ) ) ;
#9123 = LINE ( 'NONE', #24797, #15626 ) ;
#9124 = CARTESIAN_POINT ( 'NONE',  ( 38.73920764526925353, -20.11368208888610098, 72.49843995877330372 ) ) ;
#9125 = VERTEX_POINT ( 'NONE', #16482 ) ;
#9126 = ORIENTED_EDGE ( 'NONE', *, *, #25130, .T. ) ;
#9127 = CARTESIAN_POINT ( 'NONE',  ( 44.81606138205700063, 41.44123852234599781, 74.30501292736987295 ) ) ;
#9128 = CARTESIAN_POINT ( 'NONE',  ( 39.38009889167650357, -4.213682088886106847, 72.75271321436733274 ) ) ;
#9129 = CARTESIAN_POINT ( 'NONE',  ( 39.75915168707251723, -24.90384086642191619, 72.49904802271737481 ) ) ;
#9130 = CIRCLE ( 'NONE', #13246, 0.5000000000000004441 ) ;
#9131 = DIRECTION ( 'NONE',  ( -1.000000000000000000, -3.469446951953611033E-15, 0.000000000000000000 ) ) ;
#9132 = CARTESIAN_POINT ( 'NONE',  ( 39.73277004305198545, -2.213682088886108179, 73.23812341099225875 ) ) ;
#9133 = EDGE_CURVE ( 'NONE', #21411, #5237, #9706, .T. ) ;
#9134 = CARTESIAN_POINT ( 'NONE',  ( 31.56606138205697576, -5.918777154956194053, -5.916875169744970187 ) ) ;
#9135 = ADVANCED_FACE ( 'NONE', ( #10579 ), #6700, .F. ) ;
#9136 = VERTEX_POINT ( 'NONE', #20234 ) ;
#9137 = CARTESIAN_POINT ( 'NONE',  ( 40.21566563214662438, -6.564967302039574903, 83.21717579561996558 ) ) ;
#9138 = CARTESIAN_POINT ( 'NONE',  ( 46.81606138205697221, -6.425173154758061500, -4.890782882146171850 ) ) ;
#9139 = CYLINDRICAL_SURFACE ( 'NONE', #10801, 4.000000000000000000 ) ;
#9140 = CARTESIAN_POINT ( 'NONE',  ( 32.81606138205700773, -30.89740888249930961, 1.247106086993583718 ) ) ;
#9141 = CARTESIAN_POINT ( 'NONE',  ( 36.81606138205700063, 8.191238522346989015, 65.30501292736998664 ) ) ;
#9142 = AXIS2_PLACEMENT_3D ( 'NONE', #18394, #24296, #8609 ) ;
#9143 = LINE ( 'NONE', #1262, #1588 ) ;
#9144 = ORIENTED_EDGE ( 'NONE', *, *, #5659, .F. ) ;
#9145 = DIRECTION ( 'NONE',  ( 1.000000000000000000, 0.000000000000000000, -0.000000000000000000 ) ) ;
#9146 = STYLED_ITEM ( 'NONE', ( #4929 ), #17243 ) ;
#9147 = DIRECTION ( 'NONE',  ( -1.000000000000000000, -2.999999999999999839E-15, 0.000000000000000000 ) ) ;
#9148 = ORIENTED_EDGE ( 'NONE', *, *, #9177, .T. ) ;
#9149 = VERTEX_POINT ( 'NONE', #14561 ) ;
#9150 = CARTESIAN_POINT ( 'NONE',  ( 36.89935272106205133, -18.40384086642191974, 73.23812341099225875 ) ) ;
#9151 = EDGE_CURVE ( 'NONE', #2876, #2564, #2703, .T. ) ;
#9152 = CARTESIAN_POINT ( 'NONE',  ( 42.82259893474252266, 3.224890024296139135, 6.370941811568299862 ) ) ;
#9153 = CARTESIAN_POINT ( 'NONE',  ( 39.98359781491296161, -20.41368208888610525, 71.86517103874047052 ) ) ;
#9154 = CARTESIAN_POINT ( 'NONE',  ( 41.14099152588523367, 1.392818861812999964, 93.30501292736998664 ) ) ;
#9155 = ORIENTED_EDGE ( 'NONE', *, *, #3571, .F. ) ;
#9156 = CARTESIAN_POINT ( 'NONE',  ( 36.31606138205700063, 41.44123852234599781, 74.30501292736987295 ) ) ;
#9157 = CARTESIAN_POINT ( 'NONE',  ( 43.31606138205700063, -11.22674583108233115, 81.40610939240433197 ) ) ;
#9158 = CARTESIAN_POINT ( 'NONE',  ( 36.89935272106204422, -25.21368208888610241, 69.52238214136765748 ) ) ;
#9159 = VECTOR ( 'NONE', #17493, 1000.000000000000227 ) ;
#9160 = ORIENTED_EDGE ( 'NONE', *, *, #11446, .F. ) ;
#9161 = VECTOR ( 'NONE', #8881, 1000.000000000000000 ) ;
#9162 = CYLINDRICAL_SURFACE ( 'NONE', #3639, 0.7500000000000001110 ) ;
#9163 = DIRECTION ( 'NONE',  ( -0.000000000000000000, -3.469446951953613400E-15, -1.000000000000000000 ) ) ;
#9164 = CARTESIAN_POINT ( 'NONE',  ( 37.33957961208646736, 0.1863179111138910105, 72.81632618279323310 ) ) ;
#9165 = FACE_OUTER_BOUND ( 'NONE', #10096, .T. ) ;
#9166 = AXIS2_PLACEMENT_3D ( 'NONE', #18941, #10954, #5159 ) ;
#9167 = CARTESIAN_POINT ( 'NONE',  ( 36.80608444377001121, -11.31368208888610027, 70.35351908239860563 ) ) ;
#9168 = CARTESIAN_POINT ( 'NONE',  ( 32.81606138205700773, 35.92314894770294131, 80.37823623207323465 ) ) ;
#9169 = AXIS2_PLACEMENT_3D ( 'NONE', #17648, #15571, #9673 ) ;
#9170 = DIRECTION ( 'NONE',  ( 1.734723475976805122E-16, 3.491481338843134933E-15, 1.000000000000000000 ) ) ;
#9171 = CARTESIAN_POINT ( 'NONE',  ( 37.89291511884479036, -18.50384086642191406, 72.49843995877330372 ) ) ;
#9172 = CARTESIAN_POINT ( 'NONE',  ( 38.37017380507020192, -6.013682088886109334, 73.11602215082118050 ) ) ;
#9173 = ORIENTED_EDGE ( 'NONE', *, *, #7292, .F. ) ;
#9174 = DIRECTION ( 'NONE',  ( 0.000000000000000000, 1.000000000000000000, -2.643388153869420409E-15 ) ) ;
#9175 = VERTEX_POINT ( 'NONE', #12263 ) ;
#9176 = VECTOR ( 'NONE', #6648, 1000.000000000000000 ) ;
#9177 = EDGE_CURVE ( 'NONE', #10587, #24927, #19856, .T. ) ;
#9178 = CARTESIAN_POINT ( 'NONE',  ( 37.80618814713138676, -3.703840866421904909, 69.62690120949091011 ) ) ;
#9179 = PLANE ( 'NONE',  #16836 ) ;
#9180 = EDGE_CURVE ( 'NONE', #21357, #7941, #381, .T. ) ;
#9181 = VECTOR ( 'NONE', #6634, 1000.000000000000000 ) ;
#9182 = CARTESIAN_POINT ( 'NONE',  ( 38.93987200065208754, -28.81368208888610383, 70.42958956619166599 ) ) ;
#9183 = ORIENTED_EDGE ( 'NONE', *, *, #18222, .F. ) ;
#9184 = CARTESIAN_POINT ( 'NONE',  ( 40.77203464402485622, -12.51368208888610667, 71.32335560751960202 ) ) ;
#9185 = ORIENTED_EDGE ( 'NONE', *, *, #3250, .F. ) ;
#9186 = CARTESIAN_POINT ( 'NONE',  ( 30.81606138205700418, 46.92314894770293421, 79.37823623207319201 ) ) ;
#9187 = CARTESIAN_POINT ( 'NONE',  ( 39.24876120206129571, -8.903840866421910860, 72.12822762946750288 ) ) ;
#9188 = DIRECTION ( 'NONE',  ( 0.000000000000000000, 6.938893903907222067E-15, -1.000000000000000000 ) ) ;
#9189 = EDGE_LOOP ( 'NONE', ( #2656, #16819, #8665, #2961 ) ) ;
#9190 = CIRCLE ( 'NONE', #526, 1.099999999999999867 ) ;
#9191 = DIRECTION ( 'NONE',  ( 0.000000000000000000, 2.999999999999999839E-15, 1.000000000000000000 ) ) ;
#9192 = DIRECTION ( 'NONE',  ( 2.792262043613788535E-15, -0.8967398287344627850, -0.4425581086832399147 ) ) ;
#9193 = CARTESIAN_POINT ( 'NONE',  ( 40.77203464402485622, -19.10384086642191193, 71.43714994484032843 ) ) ;
#9194 = LINE ( 'NONE', #14709, #4204 ) ;
#9195 = DIRECTION ( 'NONE',  ( -1.000000000000000000, 1.040834085586084551E-30, 3.469446951953615175E-16 ) ) ;
#9196 = CARTESIAN_POINT ( 'NONE',  ( 36.68196826583682935, -19.61368208888610809, 71.96809898377888715 ) ) ;
#9197 = DIRECTION ( 'NONE',  ( 1.000000000000000000, 0.000000000000000000, 0.000000000000000000 ) ) ;
#9198 = EDGE_CURVE ( 'NONE', #10558, #19118, #17937, .T. ) ;
#9199 = CARTESIAN_POINT ( 'NONE',  ( 31.91606138205697718, -5.918777154956192277, -5.916875169744970187 ) ) ;
#9200 = CIRCLE ( 'NONE', #2165, 1.000000000000000888 ) ;
#9201 = ORIENTED_EDGE ( 'NONE', *, *, #3875, .F. ) ;
#9202 = FACE_OUTER_BOUND ( 'NONE', #24651, .T. ) ;
#9203 = CARTESIAN_POINT ( 'NONE',  ( 33.31606138205700773, 7.043113989679085307, 66.83274420321491505 ) ) ;
#9204 = VECTOR ( 'NONE', #2226, 1000.000000000000227 ) ;
#9205 = CARTESIAN_POINT ( 'NONE',  ( 39.98359781491296161, -7.203840866421913347, 70.89533451361947414 ) ) ;
#9206 = APPLICATION_PROTOCOL_DEFINITION ( 'draft international standard', 'automotive_design', 1998, #17055 ) ;
#9207 = FACE_OUTER_BOUND ( 'NONE', #14100, .T. ) ;
#9208 = CARTESIAN_POINT ( 'NONE',  ( 36.64852494920107517, -25.41368208888610525, 70.89533451361945993 ) ) ;
#9209 = DIRECTION ( 'NONE',  ( 1.000000000000000000, 0.000000000000000000, 0.000000000000000000 ) ) ;
#9210 = CIRCLE ( 'NONE', #23580, 1.000000000000000888 ) ;
#9211 = CARTESIAN_POINT ( 'NONE',  ( 38.37017380507018771, -21.60384086642190837, 69.64448340153877837 ) ) ;
#9212 = CARTESIAN_POINT ( 'NONE',  ( 37.79523030992096011, -5.268760358274976241, 83.30484586594928942 ) ) ;
#9213 = MECHANICAL_DESIGN_GEOMETRIC_PRESENTATION_REPRESENTATION (  '', ( #534 ), #24807 ) ;
#9214 = CARTESIAN_POINT ( 'NONE',  ( 39.38009889167650357, -18.21368208888610951, 72.75271321436731853 ) ) ;
#9215 = ORIENTED_EDGE ( 'NONE', *, *, #18397, .F. ) ;
#9216 = CARTESIAN_POINT ( 'NONE',  ( 40.77203464402485622, -26.51368208888610667, 71.32335560751960202 ) ) ;
#9217 = ORIENTED_EDGE ( 'NONE', *, *, #21219, .F. ) ;
#9218 = CARTESIAN_POINT ( 'NONE',  ( 33.57054579126888427, 3.412273012123826721, 6.349712035633041651 ) ) ;
#9219 = CIRCLE ( 'NONE', #3842, 0.7500000000000006661 ) ;
#9220 = DIRECTION ( 'NONE',  ( 0.000000000000000000, -4.625929269271481378E-15, -1.000000000000000000 ) ) ;
#9221 = CARTESIAN_POINT ( 'NONE',  ( 38.73920764526925353, 1.886317911113897905, 72.49843995877333214 ) ) ;
#9222 = ORIENTED_EDGE ( 'NONE', *, *, #16436, .T. ) ;
#9223 = ORIENTED_EDGE ( 'NONE', *, *, #25220, .T. ) ;
#9224 = DIRECTION ( 'NONE',  ( -1.000000000000000000, 0.000000000000000000, 0.000000000000000000 ) ) ;
#9225 = VECTOR ( 'NONE', #789, 1000.000000000000114 ) ;
#9226 = PLANE ( 'NONE',  #16141 ) ;
#9227 = ORIENTED_EDGE ( 'NONE', *, *, #6149, .T. ) ;
#9228 = PLANE ( 'NONE',  #5306 ) ;
#9229 = CARTESIAN_POINT ( 'NONE',  ( 38.93415946300896024, -3.503840866421906952, 69.66206559358663242 ) ) ;
#9230 = DIRECTION ( 'NONE',  ( 1.000000000000000000, 8.911169920151748851E-16, 3.114923731923493702E-16 ) ) ;
#9231 = AXIS2_PLACEMENT_3D ( 'NONE', #15702, #19696, #9074 ) ;
#9232 = EDGE_CURVE ( 'NONE', #12694, #22231, #24566, .T. ) ;
#9233 = LINE ( 'NONE', #22609, #9770 ) ;
#9234 = VERTEX_POINT ( 'NONE', #19986 ) ;
#9235 = ORIENTED_EDGE ( 'NONE', *, *, #19582, .T. ) ;
#9236 = DIRECTION ( 'NONE',  ( 1.000000000000000000, 2.168404344971005170E-16, -1.734723475976814737E-16 ) ) ;
#9237 = MECHANICAL_DESIGN_GEOMETRIC_PRESENTATION_REPRESENTATION (  '', ( #22379 ), #10046 ) ;
#9238 = CARTESIAN_POINT ( 'NONE',  ( 40.14115730948191185, -0.5136820888861047818, 71.32335560751961623 ) ) ;
#9239 = ORIENTED_EDGE ( 'NONE', *, *, #1823, .T. ) ;
#9240 = CARTESIAN_POINT ( 'NONE',  ( 40.04784734886185760, -29.05498820292889306, 71.69653269215241664 ) ) ;
#9241 = CIRCLE ( 'NONE', #14971, 1.500000000000001332 ) ;
#9242 = CARTESIAN_POINT ( 'NONE',  ( 43.31606138205700063, -1.963190818658398173, 19.89143565483009013 ) ) ;
#9243 = ORIENTED_EDGE ( 'NONE', *, *, #391, .T. ) ;
#9244 = DIRECTION ( 'NONE',  ( -1.000000000000000000, 0.000000000000000000, 0.000000000000000000 ) ) ;
#9245 = VECTOR ( 'NONE', #9668, 1000.000000000000000 ) ;
#9246 = CARTESIAN_POINT ( 'NONE',  ( 41.06606138205703616, -23.83075694525941302, 32.63712566015296090 ) ) ;
#9247 = CARTESIAN_POINT ( 'NONE',  ( 38.05805554829457549, -5.215892093002847396, 82.80503322521296639 ) ) ;
#9248 = ORIENTED_EDGE ( 'NONE', *, *, #11453, .T. ) ;
#9249 = CARTESIAN_POINT ( 'NONE',  ( 38.31606138205700063, -29.30876147765399864, 75.30501292736995822 ) ) ;
#9250 = ORIENTED_EDGE ( 'NONE', *, *, #20098, .T. ) ;
#9251 = ORIENTED_EDGE ( 'NONE', *, *, #9367, .F. ) ;
#9252 = FACE_OUTER_BOUND ( 'NONE', #432, .T. ) ;
#9253 = ADVANCED_BREP_SHAPE_REPRESENTATION ( '', ( #25350, #2000 ), #16613 ) ;
#9254 = DIRECTION ( 'NONE',  ( 1.000000000000000000, 0.000000000000000000, 0.000000000000000000 ) ) ;
#9255 = STYLED_ITEM ( 'NONE', ( #6112 ), #20268 ) ;
#9256 = CARTESIAN_POINT ( 'NONE',  ( 37.89291511884476904, -17.11368208888609743, 70.26206559358661252 ) ) ;
#9257 = ORIENTED_EDGE ( 'NONE', *, *, #8342, .F. ) ;
#9258 = VERTEX_POINT ( 'NONE', #20110 ) ;
#9259 = CARTESIAN_POINT ( 'NONE',  ( 38.31606138205700773, -22.27515649656512053, 29.48506754039017963 ) ) ;
#9260 = LINE ( 'NONE', #3684, #23902 ) ;
#9261 = CARTESIAN_POINT ( 'NONE',  ( 36.80608444377001831, -24.30384086642191832, 72.40698646996133903 ) ) ;
#9262 = CARTESIAN_POINT ( 'NONE',  ( 35.14099152588523367, 1.392818861812999964, 93.30501292736998664 ) ) ;
#9263 = AXIS2_PLACEMENT_3D ( 'NONE', #2600, #16514, #4308 ) ;
#9264 = EDGE_CURVE ( 'NONE', #562, #5870, #8397, .T. ) ;
#9265 = CARTESIAN_POINT ( 'NONE',  ( 36.11133435605973574, -1.613682088886104982, 72.15350918040385864 ) ) ;
#9266 = ORIENTED_EDGE ( 'NONE', *, *, #21591, .F. ) ;
#9267 = CARTESIAN_POINT ( 'NONE',  ( 43.06085722964723317, 3.410734704100585546, 6.350806999483399551 ) ) ;
#9268 = DIRECTION ( 'NONE',  ( 1.327674326049719602E-15, -0.4425581086832399147, 0.8967398287344627850 ) ) ;
#9269 = PLANE ( 'NONE',  #7505 ) ;
#9270 = CARTESIAN_POINT ( 'NONE',  ( 40.30346352106939634, -6.946260405577324271, 83.16540821620245083 ) ) ;
#9271 = DIRECTION ( 'NONE',  ( -1.000000000000000000, 0.000000000000000000, 2.507072128559814651E-16 ) ) ;
#9272 = AXIS2_PLACEMENT_3D ( 'NONE', #24987, #3108, #6986 ) ;
#9273 = PLANE ( 'NONE',  #11495 ) ;
#9274 = EDGE_CURVE ( 'NONE', #24765, #4360, #1412, .T. ) ;
#9275 = ORIENTED_EDGE ( 'NONE', *, *, #19037, .F. ) ;
#9276 = ADVANCED_FACE ( 'NONE', ( #3343 ), #1021, .T. ) ;
#9277 = CARTESIAN_POINT ( 'NONE',  ( 28.81606138205695444, -23.19619402982950263, 47.16846523730000484 ) ) ;
#9278 = CARTESIAN_POINT ( 'NONE',  ( 46.81606138205706458, -34.55876147768182705, 70.30501292735635843 ) ) ;
#9279 = ORIENTED_EDGE ( 'NONE', *, *, #20305, .T. ) ;
#9280 = ORIENTED_EDGE ( 'NONE', *, *, #5510, .F. ) ;
#9281 = CARTESIAN_POINT ( 'NONE',  ( 40.55423172469004101, -11.20384086642191690, 70.70992431699450265 ) ) ;
#9282 = EDGE_CURVE ( 'NONE', #154, #20176, #19069, .T. ) ;
#9283 = EDGE_CURVE ( 'NONE', #1959, #18383, #17137, .T. ) ;
#9284 = LINE ( 'NONE', #24349, #3364 ) ;
#9285 = CARTESIAN_POINT ( 'NONE',  ( 38.93415946300897446, -16.11368208888611164, 73.09843995877329803 ) ) ;
#9286 = CARTESIAN_POINT ( 'NONE',  ( 0.000000000000000000, 0.000000000000000000, 0.000000000000000000 ) ) ;
#9287 = EDGE_LOOP ( 'NONE', ( #10187, #20379, #6777, #14454, #9160 ) ) ;
#9288 = CARTESIAN_POINT ( 'NONE',  ( 41.31606138205700063, 3.043703737701412226, 64.67489359404071081 ) ) ;
#9289 = CARTESIAN_POINT ( 'NONE',  ( 36.31606138205700773, -19.13113579875042092, 24.60350147050422720 ) ) ;
#9290 = EDGE_CURVE ( 'NONE', #10220, #2117, #11088, .T. ) ;
#9291 = CARTESIAN_POINT ( 'NONE',  ( 36.11133435605973574, -19.61368208888610454, 72.15350918040385864 ) ) ;
#9292 = VECTOR ( 'NONE', #16607, 1000.000000000000000 ) ;
#9293 = EDGE_CURVE ( 'NONE', #2891, #16994, #22787, .T. ) ;
#9294 = VERTEX_POINT ( 'NONE', #18944 ) ;
#9295 = PLANE ( 'NONE',  #6144 ) ;
#9296 = CARTESIAN_POINT ( 'NONE',  ( 33.31606138205700773, -37.98241563432386414, 69.85268917996594951 ) ) ;
#9297 = DIRECTION ( 'NONE',  ( 0.000000000000000000, -0.8213699656732942334, 0.5703958094953462954 ) ) ;
#9298 = CARTESIAN_POINT ( 'NONE',  ( 44.81606138205700063, 39.19123852234599070, 72.05501292736988717 ) ) ;
#9299 = EDGE_CURVE ( 'NONE', #15655, #13108, #4897, .T. ) ;
#9300 = LINE ( 'NONE', #25089, #1381 ) ;
#9301 = CARTESIAN_POINT ( 'NONE',  ( 37.21915885897815457, -22.20384086642191335, 71.67976084211552745 ) ) ;
#9302 = CARTESIAN_POINT ( 'NONE',  ( 39.38009889167650357, -2.213682088886108179, 72.75271321436733274 ) ) ;
#9303 = ORIENTED_EDGE ( 'NONE', *, *, #20835, .F. ) ;
#9304 = CARTESIAN_POINT ( 'NONE',  ( 40.26596246014180736, -20.73830680248926228, 75.41253730274715394 ) ) ;
#9305 = FACE_OUTER_BOUND ( 'NONE', #5600, .T. ) ;
#9306 = ORIENTED_EDGE ( 'NONE', *, *, #18613, .T. ) ;
#9307 = ORIENTED_EDGE ( 'NONE', *, *, #2320, .T. ) ;
#9308 = CARTESIAN_POINT ( 'NONE',  ( 38.37017380507018771, -1.603840866421908595, 69.64448340153879258 ) ) ;
#9309 = FACE_OUTER_BOUND ( 'NONE', #20732, .T. ) ;
#9310 = CARTESIAN_POINT ( 'NONE',  ( 37.25202387243752611, -1.213682088886100630, 70.00779233799264034 ) ) ;
#9311 = PRODUCT ( 'Staple Magazine', 'Staple Magazine', '', ( #18979 ) ) ;
#9312 = CARTESIAN_POINT ( 'NONE',  ( 38.37017380507020192, -8.013682088886108446, 73.71602215082116061 ) ) ;
#9313 = ORIENTED_EDGE ( 'NONE', *, *, #24590, .F. ) ;
#9314 = FACE_OUTER_BOUND ( 'NONE', #21895, .T. ) ;
#9315 = CARTESIAN_POINT ( 'NONE',  ( 37.89291511884479036, -6.503840866421909617, 72.49843995877331793 ) ) ;
#9316 = LINE ( 'NONE', #19210, #5258 ) ;
#9317 = ORIENTED_EDGE ( 'NONE', *, *, #18614, .T. ) ;
#9318 = DIRECTION ( 'NONE',  ( 1.000000000000000000, 1.187136597504755470E-16, 8.249087426255173666E-17 ) ) ;
#9319 = LINE ( 'NONE', #13929, #23594 ) ;
#9320 = CARTESIAN_POINT ( 'NONE',  ( 39.12911128074872380, -7.503840866421911393, 69.06206559358666652 ) ) ;
#9321 = CARTESIAN_POINT ( 'NONE',  ( 38.05466885408097255, -22.20850960852963851, 75.30498784070806551 ) ) ;
#9322 = PRESENTATION_STYLE_ASSIGNMENT (( #10985 ) ) ;
#9323 = CARTESIAN_POINT ( 'NONE',  ( 37.69796330110504101, -23.11368208888609743, 69.66206559358660400 ) ) ;
#9324 = DIRECTION ( 'NONE',  ( -9.027796614315171564E-31, -1.000000000000000000, -3.938893903907230117E-15 ) ) ;
#9325 = CARTESIAN_POINT ( 'NONE',  ( 32.56606138205700773, 42.82479937715250173, 82.59790614618329130 ) ) ;
#9326 = EDGE_CURVE ( 'NONE', #24915, #15276, #24960, .T. ) ;
#9327 = ORIENTED_EDGE ( 'NONE', *, *, #21529, .T. ) ;
#9328 = CARTESIAN_POINT ( 'NONE',  ( 39.66066260159757917, -29.10876147765399580, 70.75778293607493197 ) ) ;
#9329 = CARTESIAN_POINT ( 'NONE',  ( 37.25202387243754032, -8.403840866421916189, 72.75271321436733274 ) ) ;
#9330 = APPLICATION_PROTOCOL_DEFINITION ( 'draft international standard', 'automotive_design', 1998, #17889 ) ;
#9331 = CARTESIAN_POINT ( 'NONE',  ( 32.81106138205699807, 3.938725376308748416, 6.271190958417212968 ) ) ;
#9332 = CARTESIAN_POINT ( 'NONE',  ( 36.49096545463212493, -25.51368208888609956, 71.43714994484030001 ) ) ;
#9333 = DIRECTION ( 'NONE',  ( -3.717264591378870232E-16, -2.999999999999999839E-15, -1.000000000000000000 ) ) ;
#9334 = CARTESIAN_POINT ( 'NONE',  ( 37.80618814713138676, -27.70384086642190269, 69.62690120949091011 ) ) ;
#9335 = CARTESIAN_POINT ( 'NONE',  ( 37.79523030992096011, -5.265685734042680366, 82.80485382125503691 ) ) ;
#9336 = CARTESIAN_POINT ( 'NONE',  ( 38.82593461698262871, -16.91368208888610170, 69.62690120949091011 ) ) ;
#9337 = ORIENTED_EDGE ( 'NONE', *, *, #409, .F. ) ;
#9338 = CARTESIAN_POINT ( 'NONE',  ( 36.98690846071097127, 0.1961591335780874246, 69.45876917294177133 ) ) ;
#9339 = ORIENTED_EDGE ( 'NONE', *, *, #18084, .T. ) ;
#9340 = PLANE ( 'NONE',  #10697 ) ;
#9341 = CARTESIAN_POINT ( 'NONE',  ( 43.81606138205700063, -25.26124097814961544, 70.06813202641110649 ) ) ;
#9342 = CARTESIAN_POINT ( 'NONE',  ( 37.12184278917507640, -26.10384086642191193, 71.32335560751960202 ) ) ;
#9343 = ORIENTED_EDGE ( 'NONE', *, *, #17612, .F. ) ;
#9344 = ORIENTED_EDGE ( 'NONE', *, *, #409, .T. ) ;
#9345 = DIRECTION ( 'NONE',  ( -0.1733269559585479680, -3.077057697073492856E-15, -0.9848643390529192576 ) ) ;
#9346 = DIRECTION ( 'NONE',  ( 0.000000000000000000, -0.8212051873014223347, -0.5706330172266899092 ) ) ;
#9347 = LINE ( 'NONE', #16939, #22156 ) ;
#9348 = CARTESIAN_POINT ( 'NONE',  ( 37.69796330110505522, -6.503840866421914058, 73.09843995877331224 ) ) ;
#9349 = DIRECTION ( 'NONE',  ( 0.000000000000000000, -0.4278636397681519488, 0.9038432971286277651 ) ) ;
#9350 = DIRECTION ( 'NONE',  ( -3.373073425510455500E-16, -2.999999999999999839E-15, -1.000000000000000000 ) ) ;
#9351 = VECTOR ( 'NONE', #25298, 1000.000000000000000 ) ;
#9352 = ORIENTED_EDGE ( 'NONE', *, *, #2275, .F. ) ;
#9353 = EDGE_CURVE ( 'NONE', #20940, #7941, #24459, .T. ) ;
#9354 = ORIENTED_EDGE ( 'NONE', *, *, #2468, .T. ) ;
#9355 = ADVANCED_FACE ( 'NONE', ( #9165 ), #14944, .F. ) ;
#9356 = CIRCLE ( 'NONE', #15087, 1.000000000000000888 ) ;
#9357 = AXIS2_PLACEMENT_3D ( 'NONE', #6467, #18446, #16756 ) ;
#9358 = CARTESIAN_POINT ( 'NONE',  ( 34.06606138205700773, -33.77966242919868733, 58.66916295099436951 ) ) ;
#9359 = CARTESIAN_POINT ( 'NONE',  ( 38.37017380507020192, -2.013682088886109334, 73.11602215082118050 ) ) ;
#9360 = CARTESIAN_POINT ( 'NONE',  ( 36.49096545463212493, -28.10384086642190837, 71.32335560751960202 ) ) ;
#9361 = CARTESIAN_POINT ( 'NONE',  ( 43.31606138205700063, -12.87480755223282358, 20.78922580900563588 ) ) ;
#9362 = VERTEX_POINT ( 'NONE', #7343 ) ;
#9363 = DIRECTION ( 'NONE',  ( 0.000000000000000000, -1.000000000000000000, 3.491481338843135327E-15 ) ) ;
#9364 = FACE_OUTER_BOUND ( 'NONE', #360, .T. ) ;
#9365 = CARTESIAN_POINT ( 'NONE',  ( 38.31606138205700773, -22.27515649656512053, 29.48506754039017963 ) ) ;
#9366 = VERTEX_POINT ( 'NONE', #24846 ) ;
#9367 = EDGE_CURVE ( 'NONE', #235, #12986, #13280, .T. ) ;
#9368 = DIRECTION ( 'NONE',  ( 2.690219486203388234E-15, -0.8967398287344627850, -0.4425581086832399147 ) ) ;
#9369 = VERTEX_POINT ( 'NONE', #12648 ) ;
#9370 = ORIENTED_EDGE ( 'NONE', *, *, #16976, .F. ) ;
#9371 = STYLED_ITEM ( 'NONE', ( #15468 ), #322 ) ;
#9372 = DIRECTION ( 'NONE',  ( -1.000000000000000000, -3.091505625455828697E-15, -4.515976121274772923E-17 ) ) ;
#9373 = CARTESIAN_POINT ( 'NONE',  ( 39.02742774030102879, -14.21368208888610241, 72.26730301774234988 ) ) ;
#9374 = AXIS2_PLACEMENT_3D ( 'NONE', #19393, #25426, #1864 ) ;
#9375 = CARTESIAN_POINT ( 'NONE',  ( 37.69225076346193504, -11.81368208888610205, 72.33091598616826445 ) ) ;
#9376 = ORIENTED_EDGE ( 'NONE', *, *, #8526, .T. ) ;
#9377 = VERTEX_POINT ( 'NONE', #7221 ) ;
#9378 = DIRECTION ( 'NONE',  ( 1.156482317317872465E-16, 0.4425581086832399702, -0.8967398287344626739 ) ) ;
#9379 = FACE_OUTER_BOUND ( 'NONE', #19717, .T. ) ;
#9380 = CARTESIAN_POINT ( 'NONE',  ( 36.80608444377001831, -22.30384086642191477, 72.40698646996135324 ) ) ;
#9381 = CARTESIAN_POINT ( 'NONE',  ( 35.31606138205687273, 43.19123852234595518, 61.30501292736988006 ) ) ;
#9382 = ORIENTED_EDGE ( 'NONE', *, *, #9662, .T. ) ;
#9383 = ORIENTED_EDGE ( 'NONE', *, *, #7075, .F. ) ;
#9384 = CARTESIAN_POINT ( 'NONE',  ( 40.64099152588522657, 1.142818861812999742, 82.55501292736997243 ) ) ;
#9385 = LINE ( 'NONE', #11325, #292 ) ;
#9386 = VECTOR ( 'NONE', #20355, 1000.000000000000000 ) ;
#9387 = CARTESIAN_POINT ( 'NONE',  ( 38.31606138205700063, -5.204193249396277032, 83.30501292736992980 ) ) ;
#9388 = AXIS2_PLACEMENT_3D ( 'NONE', #16011, #17967, #168 ) ;
#9389 = AXIS2_PLACEMENT_3D ( 'NONE', #24035, #7964, #13878 ) ;
#9390 = CARTESIAN_POINT ( 'NONE',  ( 39.64148445914975127, -5.700975119520175660, 83.29872180780533597 ) ) ;
#9391 = LINE ( 'NONE', #17237, #9824 ) ;
#9392 = DIRECTION ( 'NONE',  ( -1.000000000000000000, 0.000000000000000000, 0.000000000000000000 ) ) ;
#9393 = EDGE_LOOP ( 'NONE', ( #8607, #14361, #5163 ) ) ;
#9394 = PLANE ( 'NONE',  #17689 ) ;
#9395 = EDGE_CURVE ( 'NONE', #16417, #8890, #2950, .T. ) ;
#9396 = CARTESIAN_POINT ( 'NONE',  ( 43.31606138205700063, -29.06829118875199924, 75.80501292737000085 ) ) ;
#9397 = EDGE_LOOP ( 'NONE', ( #9086, #2010, #6970, #11908 ) ) ;
#9398 = ORIENTED_EDGE ( 'NONE', *, *, #699, .F. ) ;
#9399 = CARTESIAN_POINT ( 'NONE',  ( 39.02088643472237806, -10.70384086642192045, 73.73360434286902887 ) ) ;
#9400 = CARTESIAN_POINT ( 'NONE',  ( 36.31606138205700063, -11.65742039644129413, 17.30652615485722023 ) ) ;
#9401 = CARTESIAN_POINT ( 'NONE',  ( 39.38009889167650357, -12.21368208888610596, 72.75271321436731853 ) ) ;
#9402 = AXIS2_PLACEMENT_3D ( 'NONE', #15020, #18632, #8858 ) ;
#9403 = AXIS2_PLACEMENT_3D ( 'NONE', #19166, #17117, #1502 ) ;
#9404 = VERTEX_POINT ( 'NONE', #22801 ) ;
#9405 = DIRECTION ( 'NONE',  ( 1.000000000000000000, 1.734723475976804876E-16, -1.734723475976814737E-16 ) ) ;
#9406 = DIRECTION ( 'NONE',  ( 0.000000000000000000, 0.6568589528324746407, -0.7540134720837716742 ) ) ;
#9407 = CARTESIAN_POINT ( 'NONE',  ( 37.50301148336529167, -21.11368208888610098, 69.06206559358665231 ) ) ;
#9408 = ORIENTED_EDGE ( 'NONE', *, *, #19959, .T. ) ;
#9409 = EDGE_CURVE ( 'NONE', #17862, #19940, #5161, .T. ) ;
#9410 = CARTESIAN_POINT ( 'NONE',  ( 43.31606138205700773, -19.92642959707777806, 24.72592537066031682 ) ) ;
#9411 = CARTESIAN_POINT ( 'NONE',  ( 35.64099152588522657, 1.392818861812999964, 83.30501292736997243 ) ) ;
#9412 = CARTESIAN_POINT ( 'NONE',  ( 40.31606138205700773, -13.04008168869994577, 21.66778101221729713 ) ) ;
#9413 = EDGE_CURVE ( 'NONE', #5392, #5873, #1146, .T. ) ;
#9414 = EDGE_CURVE ( 'NONE', #18550, #3634, #11647, .T. ) ;
#9415 = ADVANCED_FACE ( 'NONE', ( #9036 ), #16881, .T. ) ;
#9416 = COLOUR_RGB ( '', 0.72549020, 0.75294118, 0.79215686) ;
#9417 = EDGE_CURVE ( 'NONE', #12220, #5555, #16146, .T. ) ;
#9418 = DIRECTION ( 'NONE',  ( -1.000000000000000000, 5.352861011585579840E-16, -1.605858303475673768E-30 ) ) ;
#9419 = DIRECTION ( 'NONE',  ( -1.000000000000000000, -2.999999999999999839E-15, 0.000000000000000000 ) ) ;
#9420 = CARTESIAN_POINT ( 'NONE',  ( 37.69225076346193504, -13.80384086642191122, 70.42958956619168021 ) ) ;
#9421 = CARTESIAN_POINT ( 'NONE',  ( 38.93415946300897446, -0.1136820888861071466, 73.09843995877331224 ) ) ;
#9422 = AXIS2_PLACEMENT_3D ( 'NONE', #18225, #8436, #12812 ) ;
#9423 = VERTEX_POINT ( 'NONE', #16615 ) ;
#9424 = LINE ( 'NONE', #17397, #15191 ) ;
#9425 = EDGE_CURVE ( 'NONE', #13947, #17020, #1327, .T. ) ;
#9426 = CARTESIAN_POINT ( 'NONE',  ( 33.31606138205700773, -11.53103574255889541, 17.35070425506816605 ) ) ;
#9427 = EDGE_LOOP ( 'NONE', ( #11920, #7548 ) ) ;
#9428 = EDGE_CURVE ( 'NONE', #13296, #4487, #23428, .T. ) ;
#9429 = VERTEX_POINT ( 'NONE', #25479 ) ;
#9430 = CARTESIAN_POINT ( 'NONE',  ( 37.61123632939164452, -27.70384086642191690, 69.02690120949091579 ) ) ;
#9431 = CARTESIAN_POINT ( 'NONE',  ( 36.80608444377001121, -1.313682088886099386, 70.35351908239860563 ) ) ;
#9432 = CARTESIAN_POINT ( 'NONE',  ( 36.36258059203031934, -1.713682088886108179, 72.86986841596736042 ) ) ;
#9433 = VERTEX_POINT ( 'NONE', #5790 ) ;
#9434 = CARTESIAN_POINT ( 'NONE',  ( 36.31606138205700063, 37.94123852234599070, 73.55501292736988717 ) ) ;
#9435 = CARTESIAN_POINT ( 'NONE',  ( 39.41296390513587511, -7.203840866421913347, 71.08074471024443142 ) ) ;
#9436 = AXIS2_PLACEMENT_3D ( 'NONE', #11198, #20591, #20465 ) ;
#9437 = CARTESIAN_POINT ( 'NONE',  ( 44.81606138205700063, -34.55876147765410167, 66.30501292737000085 ) ) ;
#9438 = ORIENTED_EDGE ( 'NONE', *, *, #7135, .T. ) ;
#9439 = CARTESIAN_POINT ( 'NONE',  ( 40.31606138205700773, -29.30876147765401640, 69.30501292737010033 ) ) ;
#9440 = DIRECTION ( 'NONE',  ( -1.000000000000000000, 5.510910596163088391E-31, 1.836970198721029688E-16 ) ) ;
#9441 = CARTESIAN_POINT ( 'NONE',  ( 40.33642880535521869, -11.30384086642191299, 69.98269868914867686 ) ) ;
#9442 = CARTESIAN_POINT ( 'NONE',  ( 37.42719827050449055, -22.01757409303136015, 75.30191050528723906 ) ) ;
#9443 = CIRCLE ( 'NONE', #8206, 0.7500000000000006661 ) ;
#9444 = DIRECTION ( 'NONE',  ( 1.327674326049719602E-15, -0.4425581086832399147, 0.8967398287344627850 ) ) ;
#9445 = SHAPE_REPRESENTATION ( 'Plastic Handle Top', ( #2000 ), #20728 ) ;
#9446 = CARTESIAN_POINT ( 'NONE',  ( 36.80608444377001121, -15.31368208888610383, 70.35351908239857721 ) ) ;
#9447 = CARTESIAN_POINT ( 'NONE',  ( 43.31606138205700773, -18.80550481115970740, 25.27912300651437150 ) ) ;
#9448 = PLANE ( 'NONE',  #17158 ) ;
#9449 = ADVANCED_FACE ( 'NONE', ( #7470 ), #15320, .T. ) ;
#9450 = VECTOR ( 'NONE', #20464, 1000.000000000000000 ) ;
#9451 = DIRECTION ( 'NONE',  ( 1.000000000000000000, 3.197344634236645231E-31, -1.734723475976814737E-16 ) ) ;
#9452 = CARTESIAN_POINT ( 'NONE',  ( 38.37017380507018771, -5.603840866421908373, 69.64448340153879258 ) ) ;
#9453 = CONTEXT_DEPENDENT_SHAPE_REPRESENTATION ( #14895, #463 ) ;
#9454 = DIRECTION ( 'NONE',  ( 0.000000000000000000, 0.8212051873014208914, 0.5706330172266919076 ) ) ;
#9455 = AXIS2_PLACEMENT_3D ( 'NONE', #12091, #12346, #2272 ) ;
#9456 = CARTESIAN_POINT ( 'NONE',  ( 36.68196826583682935, -15.61368208888610454, 71.96809898377888715 ) ) ;
#9457 = LINE ( 'NONE', #17306, #2809 ) ;
#9458 = CARTESIAN_POINT ( 'NONE',  ( 39.75915168707251723, -18.90384086642190553, 72.49904802271738902 ) ) ;
#9459 = CARTESIAN_POINT ( 'NONE',  ( 37.31005363372398165, -5.458004329937278243, 82.80203209537640419 ) ) ;
#9460 = AXIS2_PLACEMENT_3D ( 'NONE', #4128, #5804, #21514 ) ;
#9461 = CARTESIAN_POINT ( 'NONE',  ( 36.80608444377001121, -19.31368208888609672, 70.35351908239857721 ) ) ;
#9462 = EDGE_LOOP ( 'NONE', ( #15695, #20218, #2429, #1164 ) ) ;
#9463 = CARTESIAN_POINT ( 'NONE',  ( 40.55423172469004811, -22.41368208888610525, 72.05058123536544201 ) ) ;
#9464 = ORIENTED_EDGE ( 'NONE', *, *, #1692, .T. ) ;
#9465 = FACE_OUTER_BOUND ( 'NONE', #2337, .T. ) ;
#9466 = LINE ( 'NONE', #9341, #4258 ) ;
#9467 = CARTESIAN_POINT ( 'NONE',  ( 38.63098279924290068, -26.70384086642191690, 72.53360434286901182 ) ) ;
#9468 = VECTOR ( 'NONE', #11393, 1000.000000000000000 ) ;
#9469 = ORIENTED_EDGE ( 'NONE', *, *, #4050, .F. ) ;
#9470 = EDGE_CURVE ( 'NONE', #21084, #11800, #11598, .T. ) ;
#9471 = VERTEX_POINT ( 'NONE', #23170 ) ;
#9472 = DIRECTION ( 'NONE',  ( 1.000000000000000000, -8.673617379884029556E-16, 2.602085213965208662E-30 ) ) ;
#9473 = FACE_OUTER_BOUND ( 'NONE', #13668, .T. ) ;
#9474 = CARTESIAN_POINT ( 'NONE',  ( 46.81606138205707168, -35.90387122078352178, 69.64117576433150703 ) ) ;
#9475 = CARTESIAN_POINT ( 'NONE',  ( 36.07789103942399578, -26.20384086642191335, 72.05058123536544201 ) ) ;
#9476 = AXIS2_PLACEMENT_3D ( 'NONE', #9801, #13364, #21640 ) ;
#9477 = DIRECTION ( 'NONE',  ( 0.000000000000000000, -0.5706330172266920187, 0.8212051873014210024 ) ) ;
#9478 = CARTESIAN_POINT ( 'NONE',  ( 43.81606138205700063, -24.55876147765401285, 70.30501292737008612 ) ) ;
#9479 = VERTEX_POINT ( 'NONE', #3716 ) ;
#9480 = ORIENTED_EDGE ( 'NONE', *, *, #11787, .T. ) ;
#9481 = CARTESIAN_POINT ( 'NONE',  ( 34.06606138205689405, 3.151453266960317023, 6.397347472316774031 ) ) ;
#9482 = CARTESIAN_POINT ( 'NONE',  ( 36.31606138205700063, -1.357181138186128067, 82.80501292736991559 ) ) ;
#9483 = CARTESIAN_POINT ( 'NONE',  ( 37.80618814713138676, -25.70384086642190979, 69.62690120949091011 ) ) ;
#9484 = SURFACE_SIDE_STYLE ('',( #7670 ) ) ;
#9485 = DIRECTION ( 'NONE',  ( 0.000000000000000000, -1.000000000000000000, 2.999999999999999839E-15 ) ) ;
#9486 = ORIENTED_EDGE ( 'NONE', *, *, #6302, .T. ) ;
#9487 = CARTESIAN_POINT ( 'NONE',  ( 45.06606138205697221, -4.349482454670840603, -5.142398479549302515 ) ) ;
#9488 = AXIS2_PLACEMENT_3D ( 'NONE', #5266, #11066, #5394 ) ;
#9489 = CARTESIAN_POINT ( 'NONE',  ( 44.71606138205697789, -5.022037326221690634, -5.474317061061731771 ) ) ;
#9490 = DIRECTION ( 'NONE',  ( 1.734723475976804876E-16, 3.491481338843135327E-15, 1.000000000000000000 ) ) ;
#9491 = CARTESIAN_POINT ( 'NONE',  ( 39.31564783533279694, -5.303840866421911215, 70.72433947564853440 ) ) ;
#9492 = ORIENTED_EDGE ( 'NONE', *, *, #16777, .F. ) ;
#9493 = B_SPLINE_CURVE_WITH_KNOTS ( 'NONE', 3,
 ( #3786, #19010, #11540, #9481 ),
 .UNSPECIFIED., .F., .F.,
 ( 4, 4 ),
 ( 0.000000000000000000, 1.000000000000000000 ),
 .UNSPECIFIED. ) ;
#9494 = AXIS2_PLACEMENT_3D ( 'NONE', #22036, #16352, #6572 ) ;
#9495 = CARTESIAN_POINT ( 'NONE',  ( 43.31606138205700063, -35.41471100349711065, 71.53682070832086026 ) ) ;
#9496 = ORIENTED_EDGE ( 'NONE', *, *, #7536, .F. ) ;
#9497 = VERTEX_POINT ( 'NONE', #3980 ) ;
#9499 = EDGE_CURVE ( 'NONE', #5274, #24509, #13649, .T. ) ;
#9498 = CARTESIAN_POINT ( 'NONE',  ( 30.81606138205697931, -5.823060841851313008, -8.896754523299021500 ) ) ;
#9500 = CARTESIAN_POINT ( 'NONE',  ( 38.26194895904383486, -9.013682088886101340, 70.24448340153877268 ) ) ;
#9501 = ADVANCED_FACE ( 'NONE', ( #19695 ), #13402, .F. ) ;
#9502 = CARTESIAN_POINT ( 'NONE',  ( 38.26194895904383486, -13.01368208888610312, 70.24448340153875847 ) ) ;
#9503 = ORIENTED_EDGE ( 'NONE', *, *, #7895, .F. ) ;
#9504 = EDGE_CURVE ( 'NONE', #1331, #16021, #13682, .T. ) ;
#9505 = ORIENTED_EDGE ( 'NONE', *, *, #24961, .F. ) ;
#9506 = DIRECTION ( 'NONE',  ( 1.000000000000000000, -5.204170427930415223E-30, -1.734723475976805122E-15 ) ) ;
#9507 = ORIENTED_EDGE ( 'NONE', *, *, #5256, .F. ) ;
#9508 = CARTESIAN_POINT ( 'NONE',  ( 45.81606138205700063, -38.55876147765410167, 70.30501292737011454 ) ) ;
#9509 = CARTESIAN_POINT ( 'NONE',  ( 38.26194895904384907, -14.60384086642191548, 73.11602215082116629 ) ) ;
#9510 = CIRCLE ( 'NONE', #21827, 0.5000000000000004441 ) ;
#9511 = DIRECTION ( 'NONE',  ( 0.000000000000000000, 2.999999999999999839E-15, 1.000000000000000000 ) ) ;
#9512 = CARTESIAN_POINT ( 'NONE',  ( 37.38336156205274818, -15.71368208888609885, 72.12822762946750288 ) ) ;
#9513 = ORIENTED_EDGE ( 'NONE', *, *, #8562, .T. ) ;
#9514 = CIRCLE ( 'NONE', #18560, 1.550000000000002709 ) ;
#9515 = VERTEX_POINT ( 'NONE', #21503 ) ;
#9516 = DIRECTION ( 'NONE',  ( -1.327674326049719602E-15, 0.4425581086832399147, -0.8967398287344627850 ) ) ;
#9517 = EDGE_CURVE ( 'NONE', #20815, #5873, #3852, .T. ) ;
#9518 = FACE_OUTER_BOUND ( 'NONE', #18771, .T. ) ;
#9519 = CARTESIAN_POINT ( 'NONE',  ( 43.81606138205700063, 45.92314894770293421, 79.37823623207320622 ) ) ;
#9520 = CARTESIAN_POINT ( 'NONE',  ( 38.31606138205700063, -5.204193249396277032, 83.31006292736994112 ) ) ;
#9521 = CARTESIAN_POINT ( 'NONE',  ( 33.31606138205700773, -5.204193249396356968, 72.80501292736992980 ) ) ;
#9522 = B_SPLINE_SURFACE_WITH_KNOTS ( 'NONE', 1, 3, ( 
 ( #12572, #8566, #16401, #24250, #6621, #2737, #8698, #16529, #22461, #12691, #22589, #20531, #2864, #20663, #18596, #2997 ),
 ( #18731, #16791, #5452, #9335, #25129, #3513, #9459, #19358, #21046, #11267, #5705, #9710, #22844, #15237, #11518, #13567 ),
 ( #7393, #3763, #7260, #9212, #13067, #18986, #7773, #3632, #15363, #24881, #1691, #20918, #23091, #17061, #15111, #22968 ),
 ( #17437, #21291, #19116, #25264, #1326, #9586, #15487, #5205, #17561, #5331, #13322, #21174, #7646, #3258, #11388, #1455 ) ),
 .UNSPECIFIED., .F., .F., .F.,
 ( 2, 1, 1, 2 ),
 ( 4, 2, 2, 2, 2, 2, 2, 4 ),
 ( -0.01000000000000000021, 0.000000000000000000, 1.000000000000000000, 1.010099999999999998 ),
 ( 0.003138930853187265040, 0.003530919451234335038, 0.003922908049281400265, 0.004314896647328465493, 0.004706885245375529853, 0.005098873843422600284, 0.005490862441469669848, 0.006274839637563800303 ),
 .UNSPECIFIED. ) ;
#9523 = CARTESIAN_POINT ( 'NONE',  ( 40.31606138205700773, -12.76023008545320359, 21.53290024082827969 ) ) ;
#9524 = EDGE_LOOP ( 'NONE', ( #20776, #3525, #9632, #16952, #13850, #7869, #23924, #7947, #3272, #5147, #25462 ) ) ;
#9525 = AXIS2_PLACEMENT_3D ( 'NONE', #16163, #16541, #12585 ) ;
#9526 = CYLINDRICAL_SURFACE ( 'NONE', #17298, 0.7500000000000027756 ) ;
#9527 = ORIENTED_EDGE ( 'NONE', *, *, #4516, .T. ) ;
#9528 = ORIENTED_EDGE ( 'NONE', *, *, #9100, .F. ) ;
#9529 = AXIS2_PLACEMENT_3D ( 'NONE', #21094, #15159, #5506 ) ;
#9530 = CARTESIAN_POINT ( 'NONE',  ( 36.89935272106205133, -8.403840866421919742, 73.23812341099225875 ) ) ;
#9531 = CARTESIAN_POINT ( 'NONE',  ( 40.81606138205700773, -24.05876147765399864, 75.30501292737008612 ) ) ;
#9532 = CARTESIAN_POINT ( 'NONE',  ( 36.64852494920107517, -17.41368208888610525, 70.89533451361947414 ) ) ;
#9533 = ORIENTED_EDGE ( 'NONE', *, *, #14095, .F. ) ;
#9534 = LINE ( 'NONE', #15440, #15445 ) ;
#9535 = CARTESIAN_POINT ( 'NONE',  ( 31.81606138205700418, 41.44123852234599070, 73.55501292736987295 ) ) ;
#9536 = CARTESIAN_POINT ( 'NONE',  ( 37.50301148336529167, -19.11368208888609388, 69.06206559358665231 ) ) ;
#9537 = VERTEX_POINT ( 'NONE', #23293 ) ;
#9538 = CARTESIAN_POINT ( 'NONE',  ( 40.31606138205700773, -13.58280000135113319, 20.54174511886706256 ) ) ;
#9539 = CYLINDRICAL_SURFACE ( 'NONE', #25470, 1.000000000000014433 ) ;
#9540 = CARTESIAN_POINT ( 'NONE',  ( 40.31606138205700773, -11.65742039644128880, 17.30652615485722023 ) ) ;
#9541 = EDGE_CURVE ( 'NONE', #20600, #11230, #5920, .T. ) ;
#9542 = CARTESIAN_POINT ( 'NONE',  ( 36.31606138205700773, -18.80550481115971451, 25.27912300651437150 ) ) ;
#9543 = CARTESIAN_POINT ( 'NONE',  ( 40.64099152588522657, -0.6071811381869983704, 122.0250129273699997 ) ) ;
#9544 = CARTESIAN_POINT ( 'NONE',  ( 37.12184278917507640, -10.10384086642191193, 71.32335560751961623 ) ) ;
#9545 = CARTESIAN_POINT ( 'NONE',  ( 36.64852494920107517, -1.413682088886102806, 70.89533451361948835 ) ) ;
#9546 = ORIENTED_EDGE ( 'NONE', *, *, #5165, .T. ) ;
#9547 = CARTESIAN_POINT ( 'NONE',  ( 38.83857451401112826, -22.17007608312400890, 75.30462120507141321 ) ) ;
#9548 = DIRECTION ( 'NONE',  ( 9.999999999999998805E-16, -0.9439899321577399638, -0.3299742535180969494 ) ) ;
#9549 = ORIENTED_EDGE ( 'NONE', *, *, #22314, .F. ) ;
#9550 = EDGE_LOOP ( 'NONE', ( #156, #23917, #1735, #7617 ) ) ;
#9551 = CARTESIAN_POINT ( 'NONE',  ( 35.86008812008917346, -28.10384086642191903, 71.32335560751960202 ) ) ;
#9552 = ADVANCED_FACE ( 'NONE', ( #13779 ), #3473, .F. ) ;
#9553 = ADVANCED_FACE ( 'NONE', ( #11349 ), #9919, .F. ) ;
#9554 = CARTESIAN_POINT ( 'NONE',  ( 37.69225076346193504, -27.81368208888610383, 72.33091598616823603 ) ) ;
#9555 = CARTESIAN_POINT ( 'NONE',  ( 36.36258059203031934, -3.713682088886109955, 72.86986841596736042 ) ) ;
#9556 = AXIS2_PLACEMENT_3D ( 'NONE', #14000, #19793, #20047 ) ;
#9557 = ORIENTED_EDGE ( 'NONE', *, *, #14726, .F. ) ;
#9558 = FACE_OUTER_BOUND ( 'NONE', #16636, .T. ) ;
#9559 = VECTOR ( 'NONE', #11206, 1000.000000000000000 ) ;
#9560 = B_SPLINE_CURVE_WITH_KNOTS ( 'NONE', 3,
 ( #14266, #2655, #20323, #6159, #597, #19810, #20064, #2149, #715, #22118, #4226, #24042, #2276, #10030, #14145, #8472 ),
 .UNSPECIFIED., .F., .F.,
 ( 4, 2, 2, 2, 2, 2, 2, 4 ),
 ( 0.000000000000000000, 0.2499999999999884537, 0.3749999999999854006, 0.4999999999999823475, 0.6249999999999793499, 0.6874999999999815703, 0.7499999999999837907, 1.000000000000000000 ),
 .UNSPECIFIED. ) ;
#9561 = CARTESIAN_POINT ( 'NONE',  ( 37.12184278917507640, -6.103840866421912814, 71.32335560751961623 ) ) ;
#9562 = EDGE_CURVE ( 'NONE', #10558, #5367, #19192, .T. ) ;
#9563 = DIRECTION ( 'NONE',  ( -1.000000000000000000, 0.000000000000000000, 0.000000000000000000 ) ) ;
#9564 = VERTEX_POINT ( 'NONE', #9412 ) ;
#9565 = FACE_BOUND ( 'NONE', #18696, .T. ) ;
#9566 = FACE_OUTER_BOUND ( 'NONE', #4233, .T. ) ;
#9567 = VECTOR ( 'NONE', #23708, 1000.000000000000000 ) ;
#9568 = CARTESIAN_POINT ( 'NONE',  ( 37.61123632939164452, -9.703840866421911571, 69.02690120949094421 ) ) ;
#9569 = CARTESIAN_POINT ( 'NONE',  ( 43.31606138205700063, -27.25871422114667553, 59.79942265548595515 ) ) ;
#9570 = DIRECTION ( 'NONE',  ( 0.000000000000000000, 1.000000000000000000, 0.000000000000000000 ) ) ;
#9571 = CARTESIAN_POINT ( 'NONE',  ( 37.25202387243752611, -17.21368208888610241, 70.00779233799262613 ) ) ;
#9572 = CARTESIAN_POINT ( 'NONE',  ( 30.81606138205697931, -4.589472609077253296, -6.350807634294812765 ) ) ;
#9573 = ADVANCED_FACE ( 'NONE', ( #5658 ), #17260, .T. ) ;
#9574 = DIRECTION ( 'NONE',  ( -1.000000000000000000, 0.000000000000000000, 0.000000000000000000 ) ) ;
#9575 = EDGE_LOOP ( 'NONE', ( #9624, #15399, #13572, #23155 ) ) ;
#9576 = LINE ( 'NONE', #5443, #20886 ) ;
#9577 = CARTESIAN_POINT ( 'NONE',  ( 38.93415946300897446, -9.503840866421908729, 69.66206559358664663 ) ) ;
#9578 = SHAPE_DEFINITION_REPRESENTATION ( #8090, #24379 ) ;
#9579 = VECTOR ( 'NONE', #1118, 1000.000000000000114 ) ;
#9580 = CARTESIAN_POINT ( 'NONE',  ( 43.81608638205700146, 2.887189827768484207, 12.91119156276801228 ) ) ;
#9581 = CARTESIAN_POINT ( 'NONE',  ( 36.64852494920107517, -19.41368208888610525, 70.89533451361947414 ) ) ;
#9582 = DIRECTION ( 'NONE',  ( 0.000000000000000000, 0.6568589528324747517, -0.7540134720837718962 ) ) ;
#9583 = CIRCLE ( 'NONE', #18220, 0.7500000000000006661 ) ;
#9584 = CARTESIAN_POINT ( 'NONE',  ( 38.82593461698265003, -16.70384086642191690, 73.13360434286903455 ) ) ;
#9585 = EDGE_CURVE ( 'NONE', #8846, #5343, #2974, .T. ) ;
#9586 = CARTESIAN_POINT ( 'NONE',  ( 37.42710149357921523, -5.407885087272725322, 83.30820952779124866 ) ) ;
#9587 = EDGE_CURVE ( 'NONE', #8968, #7941, #7112, .T. ) ;
#9588 = B_SPLINE_CURVE_WITH_KNOTS ( 'NONE', 3,
 ( #19962, #23935, #23433, #25485 ),
 .UNSPECIFIED., .F., .F.,
 ( 4, 4 ),
 ( 0.0003110653709002429907, 1.000000000000000000 ),
 .UNSPECIFIED. ) ;
#9589 = CARTESIAN_POINT ( 'NONE',  ( 36.80608444377001121, -17.31368208888609672, 70.35351908239857721 ) ) ;
#9590 = ORIENTED_EDGE ( 'NONE', *, *, #2797, .T. ) ;
#9591 = CARTESIAN_POINT ( 'NONE',  ( 36.89935272106204422, -21.21368208888610241, 69.52238214136768590 ) ) ;
#9592 = ORIENTED_EDGE ( 'NONE', *, *, #243, .F. ) ;
#9593 = DIRECTION ( 'NONE',  ( -1.000000000000000000, 4.930380657631319405E-32, 1.734723475976804876E-16 ) ) ;
#9594 = EDGE_CURVE ( 'NONE', #25151, #5023, #17809, .T. ) ;
#9595 = CARTESIAN_POINT ( 'NONE',  ( 35.64099152588522657, -1.357181138186998925, 78.30501292736998664 ) ) ;
#9596 = CARTESIAN_POINT ( 'NONE',  ( 37.38336156205273397, -21.90384086642191619, 70.63227792289247020 ) ) ;
#9597 = ADVANCED_FACE ( 'NONE', ( #16205 ), #2288, .F. ) ;
#9598 = ADVANCED_FACE ( 'NONE', ( #18155 ), #6294, .T. ) ;
#9599 = VERTEX_POINT ( 'NONE', #13902 ) ;
#9600 = ORIENTED_EDGE ( 'NONE', *, *, #13243, .F. ) ;
#9601 = DIRECTION ( 'NONE',  ( 2.690219486203388234E-15, -0.8967398287344627850, -0.4425581086832399147 ) ) ;
#9602 = LINE ( 'NONE', #17572, #24369 ) ;
#9604 = CIRCLE ( 'NONE', #158, 0.2000000000000057288 ) ;
#9603 = DIRECTION ( 'NONE',  ( -1.000000000000000000, -2.751104698760144965E-15, 1.228345504986737969E-16 ) ) ;
#9605 = CARTESIAN_POINT ( 'NONE',  ( 36.89935272106205133, -28.40384086642191619, 73.23812341099225875 ) ) ;
#9606 = AXIS2_PLACEMENT_3D ( 'NONE', #24151, #2394, #18134 ) ;
#9607 = CARTESIAN_POINT ( 'NONE',  ( 30.81606138205698997, -30.45978664257865987, 43.58374455696577598 ) ) ;
#9608 = VECTOR ( 'NONE', #23103, 1000.000000000000000 ) ;
#9609 = CARTESIAN_POINT ( 'NONE',  ( 36.31606138205700773, -19.28757846107944474, 24.56123906878952567 ) ) ;
#9610 = ORIENTED_EDGE ( 'NONE', *, *, #20835, .T. ) ;
#9611 = ORIENTED_EDGE ( 'NONE', *, *, #17938, .T. ) ;
#9612 = DIRECTION ( 'NONE',  ( 0.1803747433772539821, 0.9835979625596982245, 0.000000000000000000 ) ) ;
#9613 = DIRECTION ( 'NONE',  ( 0.000000000000000000, -2.999999999999999839E-15, -1.000000000000000000 ) ) ;
#9614 = AXIS2_PLACEMENT_3D ( 'NONE', #18753, #16427, #8850 ) ;
#9615 = CARTESIAN_POINT ( 'NONE',  ( 40.31606138205700773, 42.19123852234596939, 66.30501292736988717 ) ) ;
#9616 = DIRECTION ( 'NONE',  ( 1.000000000000000000, 0.000000000000000000, 0.000000000000000000 ) ) ;
#9617 = EDGE_LOOP ( 'NONE', ( #15515, #13890, #18817, #23916 ) ) ;
#9618 = CARTESIAN_POINT ( 'NONE',  ( 41.31606138205700063, 3.536347952325769040, 64.10938348997790115 ) ) ;
#9619 = ADVANCED_FACE ( 'NONE', ( #20340 ), #23683, .T. ) ;
#9620 = CIRCLE ( 'NONE', #22765, 1.250000000000000888 ) ;
#9621 = LINE ( 'NONE', #5365, #7411 ) ;
#9622 = CARTESIAN_POINT ( 'NONE',  ( 31.81606138205700418, 32.99511671078946762, 63.14259751872857152 ) ) ;
#9623 = CARTESIAN_POINT ( 'NONE',  ( 39.51027997493896748, -7.103840866421911038, 71.43714994484034264 ) ) ;
#9624 = ORIENTED_EDGE ( 'NONE', *, *, #20700, .T. ) ;
#9625 = CIRCLE ( 'NONE', #7149, 1.499999999999996669 ) ;
#9626 = LINE ( 'NONE', #7808, #20202 ) ;
#9627 = ORIENTED_EDGE ( 'NONE', *, *, #22310, .T. ) ;
#9628 = VERTEX_POINT ( 'NONE', #4495 ) ;
#9629 = DIRECTION ( 'NONE',  ( 0.000000000000000000, -0.8212051873014208914, -0.5706330172266919076 ) ) ;
#9630 = CARTESIAN_POINT ( 'NONE',  ( 39.24876120206128860, -14.71368208888610241, 70.63227792289245599 ) ) ;
#9631 = CARTESIAN_POINT ( 'NONE',  ( 38.00113996487114321, -13.91368208888610347, 72.53360434286904024 ) ) ;
#9632 = ORIENTED_EDGE ( 'NONE', *, *, #12883, .F. ) ;
#9633 = AXIS2_PLACEMENT_3D ( 'NONE', #14718, #10617, #926 ) ;
#9634 = ORIENTED_EDGE ( 'NONE', *, *, #11474, .T. ) ;
#9635 = DIRECTION ( 'NONE',  ( -1.000000000000000000, -1.000000000000000078E-15, 0.000000000000000000 ) ) ;
#9636 = CARTESIAN_POINT ( 'NONE',  ( 32.81606138205700773, 22.19123852234701388, 73.80501292736992980 ) ) ;
#9637 = ORIENTED_EDGE ( 'NONE', *, *, #17291, .F. ) ;
#9638 = DIRECTION ( 'NONE',  ( 0.000000000000000000, -1.000000000000000000, 3.469446951953617344E-15 ) ) ;
#9639 = CARTESIAN_POINT ( 'NONE',  ( 38.82593461698265003, -18.70384086642191690, 73.13360434286903455 ) ) ;
#9640 = MECHANICAL_DESIGN_GEOMETRIC_PRESENTATION_REPRESENTATION (  '', ( #17438 ), #12526 ) ;
#9641 = CYLINDRICAL_SURFACE ( 'NONE', #15722, 2.500000000000002220 ) ;
#9642 = CARTESIAN_POINT ( 'NONE',  ( 38.00113996487114321, -17.91368208888609459, 72.53360434286904024 ) ) ;
#9643 = CIRCLE ( 'NONE', #8400, 10.00000000000000000 ) ;
#9644 = ORIENTED_EDGE ( 'NONE', *, *, #15572, .F. ) ;
#9645 = DIRECTION ( 'NONE',  ( -1.327674326049719602E-15, 0.4425581086832399147, -0.8967398287344627850 ) ) ;
#9646 = CARTESIAN_POINT ( 'NONE',  ( 39.29254315202756231, -16.81368208888610383, 69.94417936956672577 ) ) ;
#9647 = FACE_OUTER_BOUND ( 'NONE', #2402, .T. ) ;
#9648 = EDGE_CURVE ( 'NONE', #7819, #23131, #4621, .T. ) ;
#9649 = DIRECTION ( 'NONE',  ( -1.000000000000000000, 1.678764654171101651E-30, 5.595882180570339263E-16 ) ) ;
#9650 = EDGE_CURVE ( 'NONE', #18487, #22083, #24173, .T. ) ;
#9651 = CARTESIAN_POINT ( 'NONE',  ( 40.31606138205700773, -7.205155154158177311, 83.11773453508298815 ) ) ;
#9652 = PLANE ( 'NONE',  #10635 ) ;
#9653 = PRODUCT_DEFINITION ( 'UNKNOWN', '', #23210, #16222 ) ;
#9654 = CARTESIAN_POINT ( 'NONE',  ( 32.31606138205700063, 10.62769494289597993, 68.29765714199933768 ) ) ;
#9655 = ORIENTED_EDGE ( 'NONE', *, *, #11770, .T. ) ;
#9656 = LINE ( 'NONE', #11841, #2072 ) ;
#9657 = EDGE_LOOP ( 'NONE', ( #5514, #9869, #14429, #15375 ) ) ;
#9658 = ORIENTED_EDGE ( 'NONE', *, *, #10566, .T. ) ;
#9659 = AXIS2_PLACEMENT_3D ( 'NONE', #15630, #7529, #19617 ) ;
#9660 = CARTESIAN_POINT ( 'NONE',  ( 36.36258059203030513, -9.903840866421909084, 69.89063713639259845 ) ) ;
#9661 = ORIENTED_EDGE ( 'NONE', *, *, #14374, .T. ) ;
#9662 = EDGE_CURVE ( 'NONE', #2353, #9754, #2206, .T. ) ;
#9663 = AXIS2_PLACEMENT_3D ( 'NONE', #13960, #1585, #19504 ) ;
#9664 = DIRECTION ( 'NONE',  ( 7.071067811865491110E-16, -0.9008287146801832179, 0.4341746501209495790 ) ) ;
#9665 = CARTESIAN_POINT ( 'NONE',  ( 37.69796330110504101, -13.11368208888609743, 69.66206559358661821 ) ) ;
#9666 = ORIENTED_EDGE ( 'NONE', *, *, #3273, .T. ) ;
#9667 = CARTESIAN_POINT ( 'NONE',  ( 43.81606138205700063, -33.77966242919868733, 58.66916295099436951 ) ) ;
#9668 = DIRECTION ( 'NONE',  ( 0.000000000000000000, 1.000000000000000000, -2.913263826201159484E-15 ) ) ;
#9669 = CARTESIAN_POINT ( 'NONE',  ( 35.86008812008917346, -21.51368208888609956, 71.43714994484034264 ) ) ;
#9670 = ORIENTED_EDGE ( 'NONE', *, *, #3073, .T. ) ;
#9671 = CARTESIAN_POINT ( 'NONE',  ( 34.56606138205700773, 42.19123852234599781, 75.30501292736987295 ) ) ;
#9672 = AXIS2_PLACEMENT_3D ( 'NONE', #18847, #4939, #2730 ) ;
#9673 = DIRECTION ( 'NONE',  ( 0.000000000000000000, -0.7540134720837724513, -0.6568589528324737525 ) ) ;
#9674 = AXIS2_PLACEMENT_3D ( 'NONE', #11881, #21153, #5945 ) ;
#9675 = EDGE_CURVE ( 'NONE', #7151, #23326, #10552, .T. ) ;
#9676 = CARTESIAN_POINT ( 'NONE',  ( 31.81606138205700418, 38.19123852234598360, 71.05501292736988717 ) ) ;
#9677 = DIRECTION ( 'NONE',  ( 1.734723475976805122E-15, 2.999999999999999839E-15, 1.000000000000000000 ) ) ;
#9678 = DIRECTION ( 'NONE',  ( 0.000000000000000000, 0.000000000000000000, 1.000000000000000000 ) ) ;
#9679 = CARTESIAN_POINT ( 'NONE',  ( 39.02742774030101458, -13.40384086642191619, 70.49320253461759478 ) ) ;
#9680 = CARTESIAN_POINT ( 'NONE',  ( 36.64852494920107517, 0.5863179111138955291, 70.89533451361948835 ) ) ;
#9681 = VERTEX_POINT ( 'NONE', #20078 ) ;
#9682 = CARTESIAN_POINT ( 'NONE',  ( 39.90994555940143584, -21.47604672424653671, 75.83873687561711563 ) ) ;
#9683 = DIRECTION ( 'NONE',  ( 1.000000000000000000, -6.018531076210131309E-31, -1.734723475976804876E-16 ) ) ;
#9684 = ORIENTED_EDGE ( 'NONE', *, *, #3341, .F. ) ;
#9685 = ORIENTED_EDGE ( 'NONE', *, *, #1761, .F. ) ;
#9686 = CARTESIAN_POINT ( 'NONE',  ( 39.38009889167648936, 0.5961591335780919154, 70.00779233799265455 ) ) ;
#9687 = EDGE_CURVE ( 'NONE', #2880, #16125, #22132, .T. ) ;
#9688 = CARTESIAN_POINT ( 'NONE',  ( 38.93415946300897446, 1.886317911113891244, 73.09843995877332645 ) ) ;
#9689 = CARTESIAN_POINT ( 'NONE',  ( 36.98690846071097837, 0.1863179111138910382, 73.30173637941818754 ) ) ;
#9690 = ORIENTED_EDGE ( 'NONE', *, *, #10047, .F. ) ;
#9691 = DIRECTION ( 'NONE',  ( 1.000000000000000000, 0.000000000000000000, 0.000000000000000000 ) ) ;
#9692 = CARTESIAN_POINT ( 'NONE',  ( 38.26194895904384197, -8.603840866421911926, 72.51602215082118619 ) ) ;
#9693 = CARTESIAN_POINT ( 'NONE',  ( 33.31606138205700773, -35.70002751211045933, 71.94742330197156832 ) ) ;
#9694 = ORIENTED_EDGE ( 'NONE', *, *, #2608, .F. ) ;
#9695 = PLANE ( 'NONE',  #11330 ) ;
#9696 = DIRECTION ( 'NONE',  ( -1.000000000000000000, 0.000000000000000000, 0.000000000000000000 ) ) ;
#9697 = CARTESIAN_POINT ( 'NONE',  ( 39.02088643472237806, -12.70384086642191690, 73.73360434286898624 ) ) ;
#9698 = FACE_BOUND ( 'NONE', #5093, .T. ) ;
#9699 = FILL_AREA_STYLE ('',( #11886 ) ) ;
#9700 = CARTESIAN_POINT ( 'NONE',  ( 38.26194895904383486, -11.01368208888609956, 69.64448340153879258 ) ) ;
#9701 = DIRECTION ( 'NONE',  ( -1.000000000000000000, -1.000000000000000078E-15, 0.000000000000000000 ) ) ;
#9702 = CARTESIAN_POINT ( 'NONE',  ( 31.81606138205700418, 38.19123852234599070, 72.05501292736988717 ) ) ;
#9703 = CARTESIAN_POINT ( 'NONE',  ( 40.56606138205695800, 0.3291273985901211896, 13.05748091128652533 ) ) ;
#9704 = CARTESIAN_POINT ( 'NONE',  ( 38.82593461698264292, -4.703840866421914235, 73.13360434286904876 ) ) ;
#9705 = PLANE ( 'NONE',  #18258 ) ;
#9706 = CIRCLE ( 'NONE', #5578, 0.9999999999999937828 ) ;
#9707 = CARTESIAN_POINT ( 'NONE',  ( 40.14115730948191185, -16.51368208888610667, 71.32335560751960202 ) ) ;
#9708 = LINE ( 'NONE', #21550, #3259 ) ;
#9709 = CARTESIAN_POINT ( 'NONE',  ( 39.82603832034400426, -15.30384086642190589, 70.35351908239857721 ) ) ;
#9710 = CARTESIAN_POINT ( 'NONE',  ( 36.57819145821473228, -6.158092363301129524, 82.75995410217588244 ) ) ;
#9711 = CARTESIAN_POINT ( 'NONE',  ( 38.82593461698262871, -20.91368208888609459, 69.62690120949091011 ) ) ;
#9712 = ORIENTED_EDGE ( 'NONE', *, *, #20420, .F. ) ;
#9713 = CARTESIAN_POINT ( 'NONE',  ( 36.98690846071097837, -19.81368208888611093, 73.30173637941818754 ) ) ;
#9714 = EDGE_LOOP ( 'NONE', ( #15162, #11979, #4918, #24164 ) ) ;
#9715 = LINE ( 'NONE', #4030, #15198 ) ;
#9716 = PLANE ( 'NONE',  #11661 ) ;
#9717 = CARTESIAN_POINT ( 'NONE',  ( 39.41296390513587511, -23.20384086642191335, 71.08074471024441721 ) ) ;
#9718 = ORIENTED_EDGE ( 'NONE', *, *, #6442, .T. ) ;
#9719 = ORIENTED_EDGE ( 'NONE', *, *, #8809, .F. ) ;
#9720 = CARTESIAN_POINT ( 'NONE',  ( 33.56606138205700773, 41.44123852234599070, 73.55501292736987295 ) ) ;
#9721 = DIRECTION ( 'NONE',  ( -2.290324355028189071E-16, 0.4067366430757970996, -0.9135454576426023099 ) ) ;
#9722 = FACE_OUTER_BOUND ( 'NONE', #15910, .T. ) ;
#9723 = CARTESIAN_POINT ( 'NONE',  ( 36.29569395875881099, -28.30384086642192187, 72.77780686321126780 ) ) ;
#9724 = CARTESIAN_POINT ( 'NONE',  ( 38.26194895904383486, -1.013682088886101784, 69.04448340153881247 ) ) ;
#9725 = CARTESIAN_POINT ( 'NONE',  ( 31.81606138205700418, -38.55876147765410167, 70.30501292737011454 ) ) ;
#9726 = ORIENTED_EDGE ( 'NONE', *, *, #3907, .F. ) ;
#9727 = EDGE_CURVE ( 'NONE', #874, #4547, #6175, .T. ) ;
#9728 = ORIENTED_EDGE ( 'NONE', *, *, #22773, .T. ) ;
#9729 = CARTESIAN_POINT ( 'NONE',  ( 31.01606138205699992, 36.92314894770294131, 81.17823623207323180 ) ) ;
#9730 = ADVANCED_FACE ( 'NONE', ( #8492 ), #23803, .T. ) ;
#9731 = DIRECTION ( 'NONE',  ( -3.224213076541129652E-32, -1.000000000000000000, 2.913263826201159484E-15 ) ) ;
#9732 = ORIENTED_EDGE ( 'NONE', *, *, #16090, .T. ) ;
#9733 = CARTESIAN_POINT ( 'NONE',  ( 39.95015449827720744, -19.00384086642191406, 71.96809898377887293 ) ) ;
#9734 = ADVANCED_FACE ( 'NONE', ( #21758 ), #12116, .T. ) ;
#9735 =( NAMED_UNIT ( * ) PLANE_ANGLE_UNIT ( ) SI_UNIT ( $, .RADIAN. ) );
#9736 = DIRECTION ( 'NONE',  ( -1.734723475976804876E-16, -3.491481338843135327E-15, -1.000000000000000000 ) ) ;
#9737 = EDGE_CURVE ( 'NONE', #13895, #19743, #24354, .T. ) ;
#9738 = EDGE_CURVE ( 'NONE', #24709, #10314, #11989, .T. ) ;
#9739 = ORIENTED_EDGE ( 'NONE', *, *, #2246, .T. ) ;
#9740 = DIRECTION ( 'NONE',  ( -1.500536805400590970E-15, 0.6529557272876933549, 0.7573960774932753104 ) ) ;
#9741 = CARTESIAN_POINT ( 'NONE',  ( 38.14273442609844977, -33.30876147765400219, 70.32014858831730919 ) ) ;
#9742 = LINE ( 'NONE', #17091, #13457 ) ;
#9743 = CARTESIAN_POINT ( 'NONE',  ( 39.02742774030101458, -3.403840866421911748, 70.49320253461759478 ) ) ;
#9744 = ORIENTED_EDGE ( 'NONE', *, *, #21754, .F. ) ;
#9745 = ADVANCED_FACE ( 'NONE', ( #351 ), #10164, .T. ) ;
#9746 = PLANE ( 'NONE',  #16910 ) ;
#9747 = ORIENTED_EDGE ( 'NONE', *, *, #19638, .F. ) ;
#9748 = ORIENTED_EDGE ( 'NONE', *, *, #18945, .T. ) ;
#9749 = EDGE_CURVE ( 'NONE', #21524, #3232, #2417, .T. ) ;
#9750 = CARTESIAN_POINT ( 'NONE',  ( 45.81606138205707168, -36.80651332587431313, 65.82119181171029254 ) ) ;
#9751 = CARTESIAN_POINT ( 'NONE',  ( 37.60469502381300089, -11.21368208888610241, 70.49320253461759478 ) ) ;
#9752 = CARTESIAN_POINT ( 'NONE',  ( 37.60469502381300089, -9.213682088886100630, 70.49320253461759478 ) ) ;
#9753 = EDGE_LOOP ( 'NONE', ( #12610, #22978, #23109, #19705 ) ) ;
#9754 = VERTEX_POINT ( 'NONE', #10799 ) ;
#9755 = CARTESIAN_POINT ( 'NONE',  ( 45.81606138205697931, -8.004447042669465162, -3.950346388938982045 ) ) ;
#9756 = DIRECTION ( 'NONE',  ( 0.000000000000000000, 0.000000000000000000, -1.000000000000000000 ) ) ;
#9757 = EDGE_LOOP ( 'NONE', ( #9337, #17145, #24384, #18618 ) ) ;
#9758 = CARTESIAN_POINT ( 'NONE',  ( 39.98359781491296161, 1.586317911113896528, 71.86517103874049894 ) ) ;
#9759 = CARTESIAN_POINT ( 'NONE',  ( 38.26194895904384907, -16.60384086642191548, 73.11602215082116629 ) ) ;
#9760 = CARTESIAN_POINT ( 'NONE',  ( 40.64099152588523367, -8.607181138186998481, 78.30501292736998664 ) ) ;
#9761 = CARTESIAN_POINT ( 'NONE',  ( 37.60469502381300089, -21.21368208888610241, 70.49320253461759478 ) ) ;
#9762 = ORIENTED_EDGE ( 'NONE', *, *, #23489, .T. ) ;
#9763 = DIRECTION ( 'NONE',  ( 9.999999999999998805E-16, -0.9439899321577399638, -0.3299742535180969494 ) ) ;
#9764 = CARTESIAN_POINT ( 'NONE',  ( 36.87297107704153376, -11.71368208888611129, 72.49904802271740323 ) ) ;
#9765 = DIRECTION ( 'NONE',  ( 2.690219486203388234E-15, -0.8967398287344627850, -0.4425581086832399147 ) ) ;
#9766 = CARTESIAN_POINT ( 'NONE',  ( 43.80758608018112454, -33.17626737717533558, 59.69730689378931032 ) ) ;
#9767 = DIRECTION ( 'NONE',  ( -1.000000000000000000, 0.000000000000000000, 0.000000000000000000 ) ) ;
#9768 = DIRECTION ( 'NONE',  ( 0.000000000000000000, 1.000000000000000000, -2.775557561562891351E-15 ) ) ;
#9769 = AXIS2_PLACEMENT_3D ( 'NONE', #19343, #21407, #4014 ) ;
#9770 = VECTOR ( 'NONE', #7279, 1000.000000000000000 ) ;
#9771 = DIRECTION ( 'NONE',  ( 0.000000000000000000, -2.999999999999999839E-15, -1.000000000000000000 ) ) ;
#9772 = AXIS2_PLACEMENT_3D ( 'NONE', #9702, #23076, #17552 ) ;
#9773 = VECTOR ( 'NONE', #22430, 1000.000000000000114 ) ;
#9774 = ORIENTED_EDGE ( 'NONE', *, *, #8493, .F. ) ;
#9775 = CARTESIAN_POINT ( 'NONE',  ( 32.84131651066541480, -32.95845724189726411, 59.23979596822106686 ) ) ;
#9776 = ORIENTED_EDGE ( 'NONE', *, *, #22042, .T. ) ;
#9777 = ORIENTED_EDGE ( 'NONE', *, *, #7705, .F. ) ;
#9778 = CARTESIAN_POINT ( 'NONE',  ( 38.37017380507018771, -13.60384086642191193, 69.04448340153878405 ) ) ;
#9779 = VERTEX_POINT ( 'NONE', #12619 ) ;
#9780 = CARTESIAN_POINT ( 'NONE',  ( 40.64099152588522657, 40.39281886181299797, 84.30501292736984453 ) ) ;
#9781 = CARTESIAN_POINT ( 'NONE',  ( 38.82593461698262871, -14.91368208888609637, 69.62690120949091011 ) ) ;
#9782 = ORIENTED_EDGE ( 'NONE', *, *, #12099, .F. ) ;
#9783 = DIRECTION ( 'NONE',  ( 0.000000000000000000, 1.000000000000000000, -6.938893903907222067E-15 ) ) ;
#9784 = EDGE_CURVE ( 'NONE', #17728, #9087, #18653, .T. ) ;
#9785 = DIRECTION ( 'NONE',  ( 0.000000000000000000, -0.8212051873014208914, -0.5706330172266919076 ) ) ;
#9786 = CARTESIAN_POINT ( 'NONE',  ( 37.61123632939165873, -23.91368208888611235, 73.73360434286898624 ) ) ;
#9787 = EDGE_CURVE ( 'NONE', #828, #9062, #20458, .T. ) ;
#9788 = VECTOR ( 'NONE', #5048, 1000.000000000000000 ) ;
#9789 = VERTEX_POINT ( 'NONE', #6804 ) ;
#9790 = PLANE ( 'NONE',  #4899 ) ;
#9791 = VECTOR ( 'NONE', #5693, 1000.000000000000114 ) ;
#9792 = CIRCLE ( 'NONE', #13886, 4.000000000000000000 ) ;
#9793 = DIRECTION ( 'NONE',  ( -1.000000000000000000, -2.999999999999999839E-15, 0.000000000000000000 ) ) ;
#9794 = DIRECTION ( 'NONE',  ( -4.836319614811699678E-32, 1.000000000000000000, -3.130104260698260371E-15 ) ) ;
#9795 = CARTESIAN_POINT ( 'NONE',  ( 36.31606138205700063, 37.94123852234599781, 74.30501292736988717 ) ) ;
#9796 = CARTESIAN_POINT ( 'NONE',  ( 44.81606138205700063, -22.55876147765401996, 68.80501292737008612 ) ) ;
#9797 = CARTESIAN_POINT ( 'NONE',  ( 38.63098279924290068, -12.70384086642191157, 72.53360434286904024 ) ) ;
#9798 = CARTESIAN_POINT ( 'NONE',  ( 37.21915885897815457, -27.41368208888609814, 71.08074471024441721 ) ) ;
#9799 = ORIENTED_EDGE ( 'NONE', *, *, #14313, .F. ) ;
#9800 = PLANE ( 'NONE',  #10285 ) ;
#9801 = CARTESIAN_POINT ( 'NONE',  ( 31.81606138205700418, 38.19123852234599070, 72.05501292736988717 ) ) ;
#9802 = ORIENTED_EDGE ( 'NONE', *, *, #20730, .F. ) ;
#9803 = AXIS2_PLACEMENT_3D ( 'NONE', #753, #6822, #18797 ) ;
#9804 = ORIENTED_EDGE ( 'NONE', *, *, #14749, .F. ) ;
#9805 = CARTESIAN_POINT ( 'NONE',  ( 37.80618814713138676, -1.703840866421908018, 69.62690120949091011 ) ) ;
#9806 = CIRCLE ( 'NONE', #22534, 0.5000000000000004441 ) ;
#9807 = AXIS2_PLACEMENT_3D ( 'NONE', #10777, #6902, #4726 ) ;
#9808 = CARTESIAN_POINT ( 'NONE',  ( 39.41296390513587511, -22.41368208888610525, 71.67976084211551324 ) ) ;
#9809 = CARTESIAN_POINT ( 'NONE',  ( 39.73277004305198545, -2.213682088886108179, 73.23812341099225875 ) ) ;
#9810 = VERTEX_POINT ( 'NONE', #14653 ) ;
#9811 = CARTESIAN_POINT ( 'NONE',  ( 37.31606138205700063, 43.19123852234599070, 73.55501292736987295 ) ) ;
#9812 = CARTESIAN_POINT ( 'NONE',  ( 39.02742774030101458, -1.403840866421909972, 70.49320253461759478 ) ) ;
#9813 = EDGE_CURVE ( 'NONE', #3466, #17958, #16715, .T. ) ;
#9814 = DIRECTION ( 'NONE',  ( 1.000000000000000000, 0.000000000000000000, -0.000000000000000000 ) ) ;
#9815 = ORIENTED_EDGE ( 'NONE', *, *, #10975, .T. ) ;
#9816 = PLANE ( 'NONE',  #19134 ) ;
#9817 = ADVANCED_FACE ( 'NONE', ( #12745 ), #8616, .T. ) ;
#9818 = DIRECTION ( 'NONE',  ( -1.000000000000000000, -2.999999999999999839E-15, 0.000000000000000000 ) ) ;
#9819 = CARTESIAN_POINT ( 'NONE',  ( 40.55423172469004101, -9.203840866421915123, 70.70992431699450265 ) ) ;
#9820 = DIRECTION ( 'NONE',  ( 8.758115402030106693E-47, -1.000000000000000000, 3.469446951953613400E-15 ) ) ;
#9821 = CARTESIAN_POINT ( 'NONE',  ( 36.87297107704152666, -15.71368208888610596, 72.49904802271740323 ) ) ;
#9822 = DIRECTION ( 'NONE',  ( 1.000000000000000000, 0.000000000000000000, 0.000000000000000000 ) ) ;
#9823 = DIRECTION ( 'NONE',  ( -9.121204216617950752E-31, -0.7071067811865461294, -0.7071067811865490160 ) ) ;
#9824 = VECTOR ( 'NONE', #25063, 1000.000000000000000 ) ;
#9825 = LINE ( 'NONE', #13808, #13479 ) ;
#9826 = EDGE_CURVE ( 'NONE', #21184, #3194, #15323, .T. ) ;
#9827 = CARTESIAN_POINT ( 'NONE',  ( 39.75915168707251723, -4.903840866421915301, 72.49904802271740323 ) ) ;
#9828 = DIRECTION ( 'NONE',  ( 1.445602896647340149E-16, -0.8212051873014210024, -0.5706330172266920187 ) ) ;
#9829 = STYLED_ITEM ( 'NONE', ( #15447 ), #8398 ) ;
#9830 = CARTESIAN_POINT ( 'NONE',  ( 40.14115730948191185, -20.51368208888609601, 71.32335560751960202 ) ) ;
#9831 = LINE ( 'NONE', #5831, #16426 ) ;
#9832 = CARTESIAN_POINT ( 'NONE',  ( 39.95015449827720744, -21.00384086642191406, 71.96809898377887293 ) ) ;
#9833 = CARTESIAN_POINT ( 'NONE',  ( 29.81606138205705037, -30.46100403034036219, 72.05704881431053366 ) ) ;
#9834 = CARTESIAN_POINT ( 'NONE',  ( 39.38009889167650357, -10.21368208888610773, 72.75271321436733274 ) ) ;
#9835 = EDGE_LOOP ( 'NONE', ( #18573, #10473, #19979, #14237 ) ) ;
#9836 = CARTESIAN_POINT ( 'NONE',  ( 36.07789103942398867, -23.41368208888610525, 70.70992431699450265 ) ) ;
#9837 = ORIENTED_EDGE ( 'NONE', *, *, #20622, .T. ) ;
#9838 = FACE_OUTER_BOUND ( 'NONE', #1434, .T. ) ;
#9839 = CARTESIAN_POINT ( 'NONE',  ( 45.81606138205707168, -37.26069504592553727, 64.48189387429259511 ) ) ;
#9840 = CARTESIAN_POINT ( 'NONE',  ( 38.93987200065210175, -26.80384086642191122, 72.33091598616823603 ) ) ;
#9841 = VECTOR ( 'NONE', #18982, 1000.000000000000000 ) ;
#9842 = ORIENTED_EDGE ( 'NONE', *, *, #8155, .F. ) ;
#9843 = ORIENTED_EDGE ( 'NONE', *, *, #245, .T. ) ;
#9844 = DIRECTION ( 'NONE',  ( -1.000000000000000000, 0.000000000000000000, 1.586291242107190025E-15 ) ) ;
#9845 = CARTESIAN_POINT ( 'NONE',  ( 33.31606138205700773, -10.19550266980813724, 14.63954348514304904 ) ) ;
#9846 = ORIENTED_EDGE ( 'NONE', *, *, #7373, .T. ) ;
#9847 = PRESENTATION_STYLE_ASSIGNMENT (( #20224 ) ) ;
#9848 = CARTESIAN_POINT ( 'NONE',  ( 37.50301148336529877, -26.50384086642192116, 73.69843995877326392 ) ) ;
#9849 = DIRECTION ( 'NONE',  ( 0.000000000000000000, 1.000000000000000000, -2.999999999999999839E-15 ) ) ;
#9850 = CARTESIAN_POINT ( 'NONE',  ( 37.50301148336529167, -3.113682088886100097, 69.06206559358666652 ) ) ;
#9851 = CARTESIAN_POINT ( 'NONE',  ( 43.81608638205700146, -1.677874310045055051, 19.48083306117937852 ) ) ;
#9852 = VERTEX_POINT ( 'NONE', #15038 ) ;
#9853 = AXIS2_PLACEMENT_3D ( 'NONE', #6434, #4124, #16214 ) ;
#9854 = EDGE_LOOP ( 'NONE', ( #1729, #1659, #23027, #3181 ) ) ;
#9855 = CARTESIAN_POINT ( 'NONE',  ( 33.63257508155546560, 2.837830513113499098, 6.099065269017631685 ) ) ;
#9856 = CARTESIAN_POINT ( 'NONE',  ( 32.81606138205700773, -37.98241563432386414, 69.85268917996594951 ) ) ;
#9857 = EDGE_CURVE ( 'NONE', #21638, #7575, #4234, .T. ) ;
#9858 = CARTESIAN_POINT ( 'NONE',  ( 36.64852494920107517, -22.20384086642191335, 71.86517103874048473 ) ) ;
#9859 = DIRECTION ( 'NONE',  ( -7.966588320977881105E-33, 1.000000000000000000, -6.123233995736769734E-17 ) ) ;
#9860 = CIRCLE ( 'NONE', #20533, 0.7500000000000027756 ) ;
#9861 = EDGE_LOOP ( 'NONE', ( #23004, #8631, #10028, #20069 ) ) ;
#9862 = CARTESIAN_POINT ( 'NONE',  ( 44.81606138205700063, -36.55876147765400930, 73.30501292737011454 ) ) ;
#9863 = DIRECTION ( 'NONE',  ( 1.000000000000000000, 0.000000000000000000, -1.301042606982603842E-16 ) ) ;
#9864 = ORIENTED_EDGE ( 'NONE', *, *, #2787, .T. ) ;
#9865 = CARTESIAN_POINT ( 'NONE',  ( 39.31564783533279694, -3.303840866421912548, 70.72433947564853440 ) ) ;
#9866 = CARTESIAN_POINT ( 'NONE',  ( 43.81606138205700063, 46.92314894770294131, 81.17823623207318917 ) ) ;
#9867 = ORIENTED_EDGE ( 'NONE', *, *, #3446, .T. ) ;
#9868 = CARTESIAN_POINT ( 'NONE',  ( 39.38009889167650357, -28.21368208888610951, 72.75271321436730432 ) ) ;
#9869 = ORIENTED_EDGE ( 'NONE', *, *, #22010, .F. ) ;
#9870 = VERTEX_POINT ( 'NONE', #6670 ) ;
#9871 = LINE ( 'NONE', #9750, #18822 ) ;
#9872 = CARTESIAN_POINT ( 'NONE',  ( 37.12184278917507640, -13.51368208888610312, 71.43714994484034264 ) ) ;
#9873 = EDGE_CURVE ( 'NONE', #10709, #6775, #18623, .T. ) ;
#9874 = ADVANCED_FACE ( 'NONE', ( #14908 ), #14535, .T. ) ;
#9875 = CARTESIAN_POINT ( 'NONE',  ( 38.73920764526925353, -10.11368208888610276, 72.49843995877331793 ) ) ;
#9876 = ORIENTED_EDGE ( 'NONE', *, *, #16568, .T. ) ;
#9877 = ORIENTED_EDGE ( 'NONE', *, *, #4883, .T. ) ;
#9878 = CARTESIAN_POINT ( 'NONE',  ( 40.31606138205701484, -20.93502329652820038, 27.89939821807130826 ) ) ;
#9879 = CARTESIAN_POINT ( 'NONE',  ( 40.31606138205700773, 37.94123852234599070, 73.55501292736988717 ) ) ;
#9880 = ORIENTED_EDGE ( 'NONE', *, *, #14297, .T. ) ;
#9881 = CARTESIAN_POINT ( 'NONE',  ( 34.66606138205694521, 5.208890205473723611, 5.429380561359602453 ) ) ;
#9882 = CARTESIAN_POINT ( 'NONE',  ( 36.87297107704149823, -19.90384086642190198, 70.26145752964252722 ) ) ;
#9883 = EDGE_CURVE ( 'NONE', #18741, #12591, #23960, .T. ) ;
#9884 = EDGE_CURVE ( 'NONE', #13983, #952, #2585, .T. ) ;
#9885 = AXIS2_PLACEMENT_3D ( 'NONE', #5524, #25067, #3572 ) ;
#9886 = DIRECTION ( 'NONE',  ( -9.925461516413219746E-16, 0.8967398287344630070, 0.4425581086832393041 ) ) ;
#9887 = CARTESIAN_POINT ( 'NONE',  ( 43.81606138205700063, -35.41471100349711065, 71.53682070832086026 ) ) ;
#9888 = CARTESIAN_POINT ( 'NONE',  ( 39.31564783533280405, -16.31368208888610383, 72.03616607671141026 ) ) ;
#9889 = ORIENTED_EDGE ( 'NONE', *, *, #6269, .T. ) ;
#9890 = AXIS2_PLACEMENT_3D ( 'NONE', #14816, #18688, #16620 ) ;
#9891 = ORIENTED_EDGE ( 'NONE', *, *, #16247, .T. ) ;
#9892 = DIRECTION ( 'NONE',  ( 0.000000000000000000, 0.5706330172266907974, -0.8212051873014217795 ) ) ;
#9893 = VECTOR ( 'NONE', #3906, 1000.000000000000000 ) ;
#9894 = CARTESIAN_POINT ( 'NONE',  ( 39.29254315202756231, -14.81368208888610205, 69.94417936956672577 ) ) ;
#9895 = EDGE_CURVE ( 'NONE', #10392, #22023, #24433, .T. ) ;
#9896 = LINE ( 'NONE', #80, #16780 ) ;
#9897 = CYLINDRICAL_SURFACE ( 'NONE', #14910, 0.5000000000000004441 ) ;
#9898 = CIRCLE ( 'NONE', #25061, 0.7500000000000006661 ) ;
#9899 = CARTESIAN_POINT ( 'NONE',  ( 39.75915168707250302, -28.71368208888609175, 70.26145752964249880 ) ) ;
#9900 = CARTESIAN_POINT ( 'NONE',  ( 40.17825961694035186, -29.10876147764803079, 70.72098503771240985 ) ) ;
#9901 = CARTESIAN_POINT ( 'NONE',  ( 31.56606138205697576, -5.918777154956194053, -5.916875169744970187 ) ) ;
#9902 = ORIENTED_EDGE ( 'NONE', *, *, #4601, .T. ) ;
#9903 = CARTESIAN_POINT ( 'NONE',  ( 40.81606138205700773, 37.44123852234599781, 75.30501292736990138 ) ) ;
#9904 = EDGE_LOOP ( 'NONE', ( #1511, #15818, #24424, #18178 ) ) ;
#9905 = VERTEX_POINT ( 'NONE', #6932 ) ;
#9906 = CARTESIAN_POINT ( 'NONE',  ( 38.37017380507018771, -5.603840866421911926, 69.04448340153881247 ) ) ;
#9907 = AXIS2_PLACEMENT_3D ( 'NONE', #10855, #10728, #13036 ) ;
#9908 = EDGE_LOOP ( 'NONE', ( #9880, #15629, #23440, #15210 ) ) ;
#9909 = CARTESIAN_POINT ( 'NONE',  ( 45.81606138205700063, 44.92314894770293421, 79.37823623207320622 ) ) ;
#9910 = CARTESIAN_POINT ( 'NONE',  ( 38.93415946300897446, -10.11368208888610987, 73.09843995877331224 ) ) ;
#9911 = VECTOR ( 'NONE', #8888, 1000.000000000000000 ) ;
#9912 = EDGE_CURVE ( 'NONE', #16943, #24769, #24686, .T. ) ;
#9913 = ADVANCED_FACE ( 'NONE', ( #24814 ), #4870, .F. ) ;
#9914 = EDGE_LOOP ( 'NONE', ( #25093, #12129, #4989, #22476 ) ) ;
#9915 = DIRECTION ( 'NONE',  ( 0.1733269559585485786, 0.000000000000000000, 0.9848643390529193686 ) ) ;
#9916 = DIRECTION ( 'NONE',  ( -3.469446951953572774E-15, 0.8967398287344627850, 0.4425581086832398037 ) ) ;
#9917 = CARTESIAN_POINT ( 'NONE',  ( 36.11133435605973574, -13.61368208888610454, 72.15350918040385864 ) ) ;
#9918 = DIRECTION ( 'NONE',  ( -1.000000000000000000, -2.168404344971055214E-16, 1.734723475976814737E-16 ) ) ;
#9919 = PLANE ( 'NONE',  #17391 ) ;
#9920 = EDGE_CURVE ( 'NONE', #12702, #11458, #11444, .T. ) ;
#9921 = CARTESIAN_POINT ( 'NONE',  ( 36.31606138205700063, -31.05876147765399864, 74.30501292737010033 ) ) ;
#9922 = AXIS2_PLACEMENT_3D ( 'NONE', #9154, #11076, #8764 ) ;
#9923 = CYLINDRICAL_SURFACE ( 'NONE', #19693, 4.000000000000003553 ) ;
#9924 = DIRECTION ( 'NONE',  ( 0.000000000000000000, -1.000000000000000000, 2.999999999999999839E-15 ) ) ;
#9925 = AXIS2_PLACEMENT_3D ( 'NONE', #6531, #14390, #8094 ) ;
#9926 = CARTESIAN_POINT ( 'NONE',  ( 37.12184278917507640, -12.10384086642191193, 71.32335560751961623 ) ) ;
#9927 = CARTESIAN_POINT ( 'NONE',  ( 38.93987200065208754, -22.81368208888610383, 70.42958956619168021 ) ) ;
#9928 = ORIENTED_EDGE ( 'NONE', *, *, #2008, .F. ) ;
#9929 = EDGE_CURVE ( 'NONE', #848, #9423, #23141, .T. ) ;
#9930 = CARTESIAN_POINT ( 'NONE',  ( 42.56606138205700063, -40.21665604226827639, 68.80894170722476133 ) ) ;
#9931 = VERTEX_POINT ( 'NONE', #15676 ) ;
#9932 = ORIENTED_EDGE ( 'NONE', *, *, #4082, .F. ) ;
#9933 = CARTESIAN_POINT ( 'NONE',  ( 36.07789103942399578, -24.20384086642191690, 72.05058123536544201 ) ) ;
#9934 = CARTESIAN_POINT ( 'NONE',  ( 37.69225076346193504, -23.81368208888610027, 72.33091598616823603 ) ) ;
#9935 = PRODUCT ( 'Metal Base Plate', 'Metal Base Plate', '', ( #11261 ) ) ;
#9936 = CARTESIAN_POINT ( 'NONE',  ( 39.12911128074873801, -0.1136820888861071882, 73.69843995877330656 ) ) ;
#9937 = ORIENTED_EDGE ( 'NONE', *, *, #10147, .T. ) ;
#9938 = CYLINDRICAL_SURFACE ( 'NONE', #8265, 10.00000000000000000 ) ;
#9939 = CARTESIAN_POINT ( 'NONE',  ( 39.31564783533279694, 0.6961591335780878964, 70.72433947564853440 ) ) ;
#9940 = DIRECTION ( 'NONE',  ( 0.000000000000000000, 0.8212051873014208914, 0.5706330172266919076 ) ) ;
#9941 = ORIENTED_EDGE ( 'NONE', *, *, #5400, .T. ) ;
#9942 = FACE_BOUND ( 'NONE', #19901, .T. ) ;
#9943 = DIRECTION ( 'NONE',  ( -1.000000000000000000, 0.000000000000000000, 0.000000000000000000 ) ) ;
#9944 = CARTESIAN_POINT ( 'NONE',  ( 35.86008812008917346, -6.103840866421916367, 71.32335560751961623 ) ) ;
#9945 = VECTOR ( 'NONE', #19921, 1000.000000000000114 ) ;
#9946 = FACE_OUTER_BOUND ( 'NONE', #6255, .T. ) ;
#9947 = FILL_AREA_STYLE ('',( #3748 ) ) ;
#9948 = CARTESIAN_POINT ( 'NONE',  ( 36.80608444377001121, -11.31368208888609672, 70.35351908239857721 ) ) ;
#9949 = CARTESIAN_POINT ( 'NONE',  ( 33.77108364926073847, 2.783409424099800855, 6.088044787086559495 ) ) ;
#9950 = VECTOR ( 'NONE', #23957, 1000.000000000000000 ) ;
#9951 = CARTESIAN_POINT ( 'NONE',  ( 39.75915168707250302, -24.71368208888609885, 70.26145752964251301 ) ) ;
#9952 = CARTESIAN_POINT ( 'NONE',  ( 29.81606138205707168, -36.31746077171918330, 73.86860304758450013 ) ) ;
#9953 = CARTESIAN_POINT ( 'NONE',  ( 39.38009889167648936, -3.403840866421908196, 70.00779233799264034 ) ) ;
#9954 = ADVANCED_FACE ( 'NONE', ( #21476 ), #5390, .T. ) ;
#9955 = CARTESIAN_POINT ( 'NONE',  ( 38.09940268710882094, 38.19123852234599781, 70.07393250355386272 ) ) ;
#9956 = CARTESIAN_POINT ( 'NONE',  ( 39.95015449827720744, -18.61368208888610454, 70.79240656858105751 ) ) ;
#9957 = EDGE_CURVE ( 'NONE', #17769, #24976, #23523, .T. ) ;
#9958 = DIRECTION ( 'NONE',  ( 0.000000000000000000, -1.000000000000000000, 3.325260651745651169E-15 ) ) ;
#9959 = ADVANCED_FACE ( 'NONE', ( #5631 ), #1496, .T. ) ;
#9960 = CIRCLE ( 'NONE', #5024, 1.099999999999998312 ) ;
#9961 = CARTESIAN_POINT ( 'NONE',  ( 37.69796330110505522, -18.50384086642191406, 73.09843995877329803 ) ) ;
#9962 = CARTESIAN_POINT ( 'NONE',  ( 43.31606138205697931, -6.570990706613057064, -2.335727660491067503 ) ) ;
#9963 = VECTOR ( 'NONE', #6331, 1000.000000000000000 ) ;
#9964 = CARTESIAN_POINT ( 'NONE',  ( 39.98359781491296161, -12.41368208888610525, 71.86517103874047052 ) ) ;
#9965 = VERTEX_POINT ( 'NONE', #5760 ) ;
#9966 = CARTESIAN_POINT ( 'NONE',  ( 36.29569395875879678, -19.31368208888610027, 69.98269868914867686 ) ) ;
#9967 = VERTEX_POINT ( 'NONE', #25186 ) ;
#9968 = LINE ( 'NONE', #23220, #22618 ) ;
#9969 = CARTESIAN_POINT ( 'NONE',  ( 45.81606138205697221, -31.26685248843962839, 43.18544225915087509 ) ) ;
#9970 = CARTESIAN_POINT ( 'NONE',  ( 38.73920764526923932, -15.50384086642191228, 70.26206559358661252 ) ) ;
#9971 = ORIENTED_EDGE ( 'NONE', *, *, #20805, .T. ) ;
#9972 = EDGE_LOOP ( 'NONE', ( #9666, #11702, #13588, #18735, #10479, #4948, #16012, #5759, #1482, #21496, #11948, #25056, #7784, #6003, #3281, #161 ) ) ;
#9973 = CARTESIAN_POINT ( 'NONE',  ( 30.81606138205700418, 1.392818861812999964, 84.30501292737000085 ) ) ;
#9974 = EDGE_CURVE ( 'NONE', #13207, #6422, #6701, .T. ) ;
#9975 = LINE ( 'NONE', #9845, #21521 ) ;
#9976 = CARTESIAN_POINT ( 'NONE',  ( 36.07789103942399578, -28.20384086642191690, 72.05058123536544201 ) ) ;
#9977 = CARTESIAN_POINT ( 'NONE',  ( 34.06606138205700773, -40.21665604226827639, 68.80894170722476133 ) ) ;
#9978 = CARTESIAN_POINT ( 'NONE',  ( 35.86008812008917346, -1.513682088886105781, 71.43714994484035685 ) ) ;
#9979 = DIRECTION ( 'NONE',  ( 3.373073425510455500E-16, 2.999999999999999839E-15, 1.000000000000000000 ) ) ;
#9980 = AXIS2_PLACEMENT_3D ( 'NONE', #11577, #11833, #1623 ) ;
#9981 = ORIENTED_EDGE ( 'NONE', *, *, #23886, .F. ) ;
#9982 = ORIENTED_EDGE ( 'NONE', *, *, #6812, .T. ) ;
#9983 = LINE ( 'NONE', #6237, #3436 ) ;
#9984 = DIRECTION ( 'NONE',  ( 0.000000000000000000, 1.000000000000000000, -2.913263826201159484E-15 ) ) ;
#9985 = CARTESIAN_POINT ( 'NONE',  ( 36.87297107704151244, -21.90384086642190553, 70.26145752964255564 ) ) ;
#9986 = CARTESIAN_POINT ( 'NONE',  ( 33.31606138205700773, 2.715274261285174351, 65.05190033008260286 ) ) ;
#9987 = VERTEX_POINT ( 'NONE', #17233 ) ;
#9988 = CARTESIAN_POINT ( 'NONE',  ( 43.31606138205700063, -33.60910547091194900, 60.61426200347987248 ) ) ;
#9989 = VECTOR ( 'NONE', #993, 1000.000000000000227 ) ;
#9990 = CIRCLE ( 'NONE', #24358, 1.999999999999999778 ) ;
#9991 = CARTESIAN_POINT ( 'NONE',  ( 40.81606138205700773, -24.05876147765399864, 75.30501292737008612 ) ) ;
#9992 = ORIENTED_EDGE ( 'NONE', *, *, #21858, .F. ) ;
#9993 = CARTESIAN_POINT ( 'NONE',  ( 38.37017380507018771, -7.603840866421910150, 70.24448340153877268 ) ) ;
#9994 = ORIENTED_EDGE ( 'NONE', *, *, #17987, .F. ) ;
#9995 = FACE_OUTER_BOUND ( 'NONE', #19170, .T. ) ;
#9996 = ORIENTED_EDGE ( 'NONE', *, *, #9541, .T. ) ;
#9997 = ORIENTED_EDGE ( 'NONE', *, *, #11134, .F. ) ;
#9998 = VECTOR ( 'NONE', #2105, 1000.000000000000000 ) ;
#9999 = CARTESIAN_POINT ( 'NONE',  ( 43.31606138205700773, -21.24830114143971116, 28.89343865514767273 ) ) ;
#10000 = CARTESIAN_POINT ( 'NONE',  ( 37.12184278917507640, -5.513682088886102228, 71.43714994484035685 ) ) ;
#10001 = CARTESIAN_POINT ( 'NONE',  ( 37.89291511884476904, -5.113682088886100985, 70.26206559358664094 ) ) ;
#10002 = ORIENTED_EDGE ( 'NONE', *, *, #21536, .F. ) ;
#10003 = ORIENTED_EDGE ( 'NONE', *, *, #5950, .T. ) ;
#10004 = DIRECTION ( 'NONE',  ( 4.425581086832455372E-16, -0.4425581086832455213, 0.8967398287344600094 ) ) ;
#10005 = ADVANCED_FACE ( 'NONE', ( #7443 ), #19040, .F. ) ;
#10006 = AXIS2_PLACEMENT_3D ( 'NONE', #4554, #2347, #408 ) ;
#10007 = CARTESIAN_POINT ( 'NONE',  ( 30.81606138205700418, 44.92314894770293421, 79.37823623207320622 ) ) ;
#10008 = ORIENTED_EDGE ( 'NONE', *, *, #22773, .F. ) ;
#10009 = DIRECTION ( 'NONE',  ( -1.000000000000000078E-15, 0.9439899321577400748, 0.3299742535180970049 ) ) ;
#10010 = CARTESIAN_POINT ( 'NONE',  ( 39.95015449827720744, -15.00384086642191228, 71.96809898377887293 ) ) ;
#10011 = CARTESIAN_POINT ( 'NONE',  ( 37.09113907096683960, -21.82868160544892788, 75.81787431707023472 ) ) ;
#10012 = AXIS2_PLACEMENT_3D ( 'NONE', #13249, #9516, #23273 ) ;
#10013 = LINE ( 'NONE', #10610, #18629 ) ;
#10014 = CARTESIAN_POINT ( 'NONE',  ( 39.41296390513587511, -18.41368208888610170, 71.67976084211551324 ) ) ;
#10015 = ORIENTED_EDGE ( 'NONE', *, *, #4238, .F. ) ;
#10016 = ORIENTED_EDGE ( 'NONE', *, *, #25372, .T. ) ;
#10017 = DIRECTION ( 'NONE',  ( -1.000000000000000000, 0.000000000000000000, 0.000000000000000000 ) ) ;
#10018 = CARTESIAN_POINT ( 'NONE',  ( 38.37017380507020192, -16.01368208888610667, 73.11602215082116629 ) ) ;
#10019 = AXIS2_PLACEMENT_3D ( 'NONE', #944, #18992, #9220 ) ;
#10020 = DIRECTION ( 'NONE',  ( 0.000000000000000000, 1.000000000000000000, -3.469446951953614189E-15 ) ) ;
#10021 = VECTOR ( 'NONE', #9859, 1000.000000000000000 ) ;
#10022 = CARTESIAN_POINT ( 'NONE',  ( 43.31606138205700063, 3.195231713396695650, 64.80689721350518084 ) ) ;
#10023 = DIRECTION ( 'NONE',  ( -1.000000000000000000, 1.301042606982604506E-30, 4.336808689942015271E-16 ) ) ;
#10024 = DIRECTION ( 'NONE',  ( 0.000000000000000000, 2.999999999999999839E-15, 1.000000000000000000 ) ) ;
#10025 = CIRCLE ( 'NONE', #8791, 0.7500000000000006661 ) ;
#10026 = LINE ( 'NONE', #16061, #10702 ) ;
#10027 = DIRECTION ( 'NONE',  ( -1.000000000000000000, 5.204170427930415223E-30, 1.734723475976805122E-15 ) ) ;
#10028 = ORIENTED_EDGE ( 'NONE', *, *, #11318, .T. ) ;
#10029 = AXIS2_PLACEMENT_3D ( 'NONE', #25287, #13462, #17585 ) ;
#10030 = CARTESIAN_POINT ( 'NONE',  ( 37.79221860075193717, -22.16980752718048464, 75.30461792607815141 ) ) ;
#10031 = ORIENTED_EDGE ( 'NONE', *, *, #12418, .F. ) ;
#10032 = ORIENTED_EDGE ( 'NONE', *, *, #3567, .T. ) ;
#10033 = CARTESIAN_POINT ( 'NONE',  ( 39.64521430340305841, -2.803840866421918765, 73.30173637941818754 ) ) ;
#10034 = ORIENTED_EDGE ( 'NONE', *, *, #16044, .F. ) ;
#10035 = PLANE ( 'NONE',  #22283 ) ;
#10036 = CARTESIAN_POINT ( 'NONE',  ( 39.29254315202756231, -10.81368208888610205, 69.94417936956673998 ) ) ;
#10037 = VECTOR ( 'NONE', #3157, 1000.000000000000000 ) ;
#10038 = ORIENTED_EDGE ( 'NONE', *, *, #13879, .T. ) ;
#10039 = CARTESIAN_POINT ( 'NONE',  ( 44.06606138205700063, 40.39281886181299797, 84.30501292736984453 ) ) ;
#10040 = CIRCLE ( 'NONE', #23618, 0.7500000000000001110 ) ;
#10041 = CARTESIAN_POINT ( 'NONE',  ( 37.61123632939165873, -13.91368208888610525, 73.73360434286898624 ) ) ;
#10042 = CARTESIAN_POINT ( 'NONE',  ( 40.81606138205700773, -24.05876147765399864, 75.30501292737008612 ) ) ;
#10043 = CARTESIAN_POINT ( 'NONE',  ( 1.805559322863034488E-31, -29.10876147765387856, -4.761918834291073356E-14 ) ) ;
#10044 = CARTESIAN_POINT ( 'NONE',  ( 39.62658885603860881, -28.92295460646453265, 69.87450580589076310 ) ) ;
#10045 = EDGE_CURVE ( 'NONE', #22094, #21036, #17496, .T. ) ;
#10046 =( GEOMETRIC_REPRESENTATION_CONTEXT ( 3 ) GLOBAL_UNCERTAINTY_ASSIGNED_CONTEXT ( ( #8761 ) ) GLOBAL_UNIT_ASSIGNED_CONTEXT ( ( #21579, #9735, #11674 ) ) REPRESENTATION_CONTEXT ( 'NONE', 'WORKASPACE' ) );
#10047 = EDGE_CURVE ( 'NONE', #9628, #9599, #23973, .T. ) ;
#10048 = DIRECTION ( 'NONE',  ( 1.734723475976805517E-15, -0.4425581086832399702, 0.8967398287344627850 ) ) ;
#10049 = EDGE_CURVE ( 'NONE', #18694, #7382, #18642, .T. ) ;
#10050 = AXIS2_PLACEMENT_3D ( 'NONE', #9720, #2093, #25276 ) ;
#10051 = AXIS2_PLACEMENT_3D ( 'NONE', #20410, #21967, #12449 ) ;
#10052 = DIRECTION ( 'NONE',  ( 0.000000000000000000, -0.7516416929448823669, -0.6595716529892345914 ) ) ;
#10053 = EDGE_CURVE ( 'NONE', #18026, #24670, #24929, .T. ) ;
#10054 = CYLINDRICAL_SURFACE ( 'NONE', #3249, 2.500000000000002220 ) ;
#10055 = CARTESIAN_POINT ( 'NONE',  ( 38.37017380507020192, -24.01368208888609956, 72.51602215082114355 ) ) ;
#10056 = ADVANCED_FACE ( 'NONE', ( #13754 ), #1879, .T. ) ;
#10057 = ORIENTED_EDGE ( 'NONE', *, *, #3250, .T. ) ;
#10058 = LINE ( 'NONE', #19444, #4921 ) ;
#10059 = AXIS2_PLACEMENT_3D ( 'NONE', #14746, #7412, #11149 ) ;
#10060 = DIRECTION ( 'NONE',  ( -1.225631768639319301E-15, 0.4425581086832399147, -0.8967398287344627850 ) ) ;
#10061 = VERTEX_POINT ( 'NONE', #25450 ) ;
#10062 = ORIENTED_EDGE ( 'NONE', *, *, #4964, .F. ) ;
#10063 = CARTESIAN_POINT ( 'NONE',  ( 36.29569395875881099, -26.30384086642192187, 72.77780686321126780 ) ) ;
#10064 = EDGE_CURVE ( 'NONE', #8849, #6796, #12899, .T. ) ;
#10065 = CARTESIAN_POINT ( 'NONE',  ( 37.25202387243752611, -27.21368208888610241, 70.00779233799262613 ) ) ;
#10066 = CARTESIAN_POINT ( 'NONE',  ( 43.31606138205700063, -16.48551471403133206, 77.11349248448009064 ) ) ;
#10067 = EDGE_CURVE ( 'NONE', #24915, #2564, #13493, .T. ) ;
#10068 = CARTESIAN_POINT ( 'NONE',  ( 38.26194895904384197, -0.6038408664219111488, 72.51602215082118619 ) ) ;
#10069 = AXIS2_PLACEMENT_3D ( 'NONE', #12807, #22455, #2991 ) ;
#10070 = PLANE ( 'NONE',  #4845 ) ;
#10071 = ORIENTED_EDGE ( 'NONE', *, *, #4374, .F. ) ;
#10072 = CARTESIAN_POINT ( 'NONE',  ( 40.31606138205700063, -6.980777400833622970, 82.64680122081715297 ) ) ;
#10073 = DIRECTION ( 'NONE',  ( 0.000000000000000000, -1.000000000000000000, 2.643388153869420804E-15 ) ) ;
#10074 = CARTESIAN_POINT ( 'NONE',  ( 38.26194895904384197, -6.603840866421920808, 73.71602215082116061 ) ) ;
#10075 = AXIS2_PLACEMENT_3D ( 'NONE', #17571, #9601, #6099 ) ;
#10076 = CARTESIAN_POINT ( 'NONE',  ( 45.06606138205697931, -5.918777154956152309, -5.916875169744970187 ) ) ;
#10077 = CYLINDRICAL_SURFACE ( 'NONE', #15287, 0.4999999999999994449 ) ;
#10078 = CARTESIAN_POINT ( 'NONE',  ( 39.98359781491296161, -10.41368208888610347, 71.86517103874048473 ) ) ;
#10079 = CARTESIAN_POINT ( 'NONE',  ( 33.31606138205700773, 2.715274261285174351, 65.05190033008260286 ) ) ;
#10080 = ADVANCED_FACE ( 'NONE', ( #1383 ), #20178, .T. ) ;
#10081 = CARTESIAN_POINT ( 'NONE',  ( 40.14115730948191185, -24.51368208888610312, 71.32335560751960202 ) ) ;
#10082 = VECTOR ( 'NONE', #11253, 1000.000000000000000 ) ;
#10083 = CARTESIAN_POINT ( 'NONE',  ( 45.81606138205705747, -33.21365173458013231, 70.96885009038120984 ) ) ;
#10084 = CARTESIAN_POINT ( 'NONE',  ( 38.82593461698264292, -0.7038408664219141242, 73.13360434286904876 ) ) ;
#10085 = DIRECTION ( 'NONE',  ( 0.000000000000000000, -0.3299742535180974490, 0.9439899321577398528 ) ) ;
#10086 = CARTESIAN_POINT ( 'NONE',  ( 37.60469502381300799, -26.40384086642190908, 72.26730301774232146 ) ) ;
#10087 = CARTESIAN_POINT ( 'NONE',  ( 38.82593461698262871, -14.91368208888609637, 69.62690120949091011 ) ) ;
#10088 = DIRECTION ( 'NONE',  ( 1.000000000000000000, -1.301042606982604506E-30, -4.336808689942015271E-16 ) ) ;
#10089 = VECTOR ( 'NONE', #22693, 1000.000000000000000 ) ;
#10090 = CARTESIAN_POINT ( 'NONE',  ( 36.87297107704149823, -11.90384086642190731, 70.26145752964252722 ) ) ;
#10091 = AXIS2_PLACEMENT_3D ( 'NONE', #1812, #13428, #19468 ) ;
#10092 = LINE ( 'NONE', #6216, #18808 ) ;
#10093 = CARTESIAN_POINT ( 'NONE',  ( 37.80618814713140097, -11.91368208888611058, 73.13360434286903455 ) ) ;
#10094 = ORIENTED_EDGE ( 'NONE', *, *, #3190, .F. ) ;
#10095 = CARTESIAN_POINT ( 'NONE',  ( 40.52078840805428683, -18.61368208888610098, 70.60699637195608602 ) ) ;
#10096 = EDGE_LOOP ( 'NONE', ( #16643, #15844, #15923, #13219 ) ) ;
#10097 = CARTESIAN_POINT ( 'NONE',  ( 40.31606138205700063, 5.691238522346998785, 68.80501292736998664 ) ) ;
#10098 = CARTESIAN_POINT ( 'NONE',  ( 28.81606138205696155, 0.8576245772853319238, -1.570935883000529332 ) ) ;
#10099 = CARTESIAN_POINT ( 'NONE',  ( 38.63098279924290068, -20.70384086642191335, 72.53360434286904024 ) ) ;
#10100 = ORIENTED_EDGE ( 'NONE', *, *, #18080, .T. ) ;
#10101 = ORIENTED_EDGE ( 'NONE', *, *, #10045, .T. ) ;
#10102 = DIRECTION ( 'NONE',  ( -1.000000000000000000, -1.956963323498894821E-16, 5.870889970496684443E-31 ) ) ;
#10103 = CARTESIAN_POINT ( 'NONE',  ( 43.31606138205700773, -22.71854986786758701, 31.51329497139233737 ) ) ;
#10104 = CARTESIAN_POINT ( 'NONE',  ( 36.36258059203030513, -19.90384086642191264, 69.89063713639259845 ) ) ;
#10105 = FACE_OUTER_BOUND ( 'NONE', #9757, .T. ) ;
#10106 = CARTESIAN_POINT ( 'NONE',  ( 40.52078840805428683, 1.386317911113894130, 70.60699637195612866 ) ) ;
#10107 = PRODUCT_DEFINITION ( 'UNKNOWN', '', #18289, #5907 ) ;
#10108 = DIRECTION ( 'NONE',  ( 1.000000000000000000, 0.000000000000000000, 0.000000000000000000 ) ) ;
#10109 = VECTOR ( 'NONE', #18677, 1000.000000000000000 ) ;
#10110 = VERTEX_POINT ( 'NONE', #10267 ) ;
#10111 = DIRECTION ( 'NONE',  ( 2.792262043613788535E-15, -0.8967398287344627850, -0.4425581086832398592 ) ) ;
#10112 = FACE_OUTER_BOUND ( 'NONE', #9835, .T. ) ;
#10113 = CARTESIAN_POINT ( 'NONE',  ( 36.87297107704151244, -23.90384086642190553, 70.26145752964252722 ) ) ;
#10114 = DIRECTION ( 'NONE',  ( -1.327674326049719602E-15, 0.4425581086832399147, -0.8967398287344627850 ) ) ;
#10115 = ORIENTED_EDGE ( 'NONE', *, *, #9895, .F. ) ;
#10116 = LINE ( 'NONE', #12307, #8184 ) ;
#10117 = LINE ( 'NONE', #16148, #10684 ) ;
#10118 = CARTESIAN_POINT ( 'NONE',  ( 38.73920764526923932, -1.503840866421912725, 70.26206559358664094 ) ) ;
#10119 = DIRECTION ( 'NONE',  ( 0.000000000000000000, 1.000000000000000000, -2.999999999999999839E-15 ) ) ;
#10120 = ORIENTED_EDGE ( 'NONE', *, *, #25442, .F. ) ;
#10121 = CARTESIAN_POINT ( 'NONE',  ( 38.82593461698262871, -28.91368208888610525, 69.62690120949091011 ) ) ;
#10122 = EDGE_LOOP ( 'NONE', ( #10694, #5466, #17396, #16671 ) ) ;
#10123 = VERTEX_POINT ( 'NONE', #13876 ) ;
#10124 = CARTESIAN_POINT ( 'NONE',  ( 36.31606138205700773, -21.45740613484710835, 28.95788407061096237 ) ) ;
#10125 = CARTESIAN_POINT ( 'NONE',  ( 46.81606138205706458, -34.55876147768182705, 70.30501292735635843 ) ) ;
#10126 = CARTESIAN_POINT ( 'NONE',  ( 38.73920764526925353, -6.113682088886101873, 72.49843995877331793 ) ) ;
#10127 = CARTESIAN_POINT ( 'NONE',  ( 39.41296390513587511, -2.413682088886099919, 71.67976084211552745 ) ) ;
#10128 = ORIENTED_EDGE ( 'NONE', *, *, #21241, .T. ) ;
#10129 = ORIENTED_EDGE ( 'NONE', *, *, #6807, .T. ) ;
#10130 = CARTESIAN_POINT ( 'NONE',  ( 32.81606138205700773, -33.70281195181703993, 69.07320514641659770 ) ) ;
#10131 = DIRECTION ( 'NONE',  ( 0.000000000000000000, 1.000000000000000000, -2.999999999999999839E-15 ) ) ;
#10132 = VERTEX_POINT ( 'NONE', #22233 ) ;
#10133 = LINE ( 'NONE', #17994, #13637 ) ;
#10134 = CARTESIAN_POINT ( 'NONE',  ( 38.82593461698265003, -8.703840866421909794, 73.13360434286904876 ) ) ;
#10135 = EDGE_CURVE ( 'NONE', #8061, #10587, #18130, .T. ) ;
#10136 = EDGE_CURVE ( 'NONE', #4880, #22885, #24374, .T. ) ;
#10137 = CARTESIAN_POINT ( 'NONE',  ( 35.56606138205703616, -23.83075694525942723, 32.63712566015296090 ) ) ;
#10138 = DIRECTION ( 'NONE',  ( 7.071067811865460542E-16, -0.4341746501209495790, -0.9008287146801832179 ) ) ;
#10139 = ORIENTED_EDGE ( 'NONE', *, *, #11804, .T. ) ;
#10140 = VERTEX_POINT ( 'NONE', #17880 ) ;
#10141 = DIRECTION ( 'NONE',  ( 0.000000000000000000, 0.1918498038142811835, -0.9814242980364923374 ) ) ;
#10142 = CARTESIAN_POINT ( 'NONE',  ( 37.33957961208646736, -9.813682088886107380, 72.81632618279323310 ) ) ;
#10143 = DIRECTION ( 'NONE',  ( 0.000000000000000000, -0.4278636397681519488, 0.9038432971286277651 ) ) ;
#10144 = CARTESIAN_POINT ( 'NONE',  ( 43.31606138205697221, -3.118133360756952577, 16.65315793475036443 ) ) ;
#10145 = CARTESIAN_POINT ( 'NONE',  ( 43.81606138205700063, 46.72314894770294558, 81.37823623207320622 ) ) ;
#10146 = LINE ( 'NONE', #4351, #7334 ) ;
#10147 = EDGE_CURVE ( 'NONE', #2806, #18113, #12082, .T. ) ;
#10148 = PRODUCT ( 'Follower', 'Follower', '', ( #21283 ) ) ;
#10149 = CARTESIAN_POINT ( 'NONE',  ( 28.81606138205695444, -23.19619402982950263, 47.16846523730000484 ) ) ;
#10150 = CARTESIAN_POINT ( 'NONE',  ( 33.31606138205700773, 9.119667998728431257, 66.98393923633439329 ) ) ;
#10151 = ORIENTED_EDGE ( 'NONE', *, *, #13378, .T. ) ;
#10152 = DIRECTION ( 'NONE',  ( 0.000000000000000000, 1.000000000000000000, -2.999999999999999839E-15 ) ) ;
#10153 = ORIENTED_EDGE ( 'NONE', *, *, #7051, .F. ) ;
#10154 = ORIENTED_EDGE ( 'NONE', *, *, #1042, .T. ) ;
#10155 = DIRECTION ( 'NONE',  ( -1.000000000000000000, -1.185941393278724777E-16, -8.240782279085522416E-17 ) ) ;
#10156 = CARTESIAN_POINT ( 'NONE',  ( 40.52078840805429394, -7.003840866421914058, 72.15350918040385864 ) ) ;
#10157 = ORIENTED_EDGE ( 'NONE', *, *, #21733, .T. ) ;
#10158 = DIRECTION ( 'NONE',  ( 1.218693434051482139E-16, -0.4425581086832393041, 0.8967398287344630070 ) ) ;
#10159 = CARTESIAN_POINT ( 'NONE',  ( 39.95015449827720744, -10.61368208888610631, 70.79240656858107172 ) ) ;
#10160 = VERTEX_POINT ( 'NONE', #2012 ) ;
#10161 = LINE ( 'NONE', #14028, #7521 ) ;
#10162 = CARTESIAN_POINT ( 'NONE',  ( 36.07789103942398867, -17.41368208888610525, 70.70992431699450265 ) ) ;
#10163 = LINE ( 'NONE', #4245, #6975 ) ;
#10164 = CYLINDRICAL_SURFACE ( 'NONE', #20689, 0.5000000000000004441 ) ;
#10165 = CARTESIAN_POINT ( 'NONE',  ( 43.30787617916693932, 3.971823716557246975, 6.337422814852420316 ) ) ;
#10166 = AXIS2_PLACEMENT_3D ( 'NONE', #2609, #4436, #12302 ) ;
#10167 = CIRCLE ( 'NONE', #23723, 0.9999999999999937828 ) ;
#10168 = CARTESIAN_POINT ( 'NONE',  ( 32.81606138205700773, -2.373793412309109563, 19.60611914621674146 ) ) ;
#10169 = EDGE_CURVE ( 'NONE', #13134, #25424, #205, .T. ) ;
#10170 = FACE_OUTER_BOUND ( 'NONE', #14492, .T. ) ;
#10171 = LINE ( 'NONE', #18163, #5725 ) ;
#10172 = CARTESIAN_POINT ( 'NONE',  ( 38.73920764526925353, -26.11368208888610454, 72.49843995877328950 ) ) ;
#10173 = ORIENTED_EDGE ( 'NONE', *, *, #16919, .T. ) ;
#10174 = CARTESIAN_POINT ( 'NONE',  ( 39.20536636138601949, -22.02770764502952616, 75.80686379705316824 ) ) ;
#10175 = CARTESIAN_POINT ( 'NONE',  ( 38.31606138205700063, 38.69123852234597649, 69.30501292736988717 ) ) ;
#10176 = ORIENTED_EDGE ( 'NONE', *, *, #11549, .T. ) ;
#10177 = ORIENTED_EDGE ( 'NONE', *, *, #10516, .F. ) ;
#10178 = CARTESIAN_POINT ( 'NONE',  ( 40.55423172469004101, -21.20384086642191690, 70.70992431699450265 ) ) ;
#10179 = CARTESIAN_POINT ( 'NONE',  ( 36.49096545463212493, -25.51368208888609956, 71.43714994484030001 ) ) ;
#10180 = CARTESIAN_POINT ( 'NONE',  ( 43.81608638205700146, -1.677874310045055051, 19.48083306117937852 ) ) ;
#10181 = VECTOR ( 'NONE', #1801, 1000.000000000000000 ) ;
#10182 = EDGE_CURVE ( 'NONE', #25304, #19848, #10428, .T. ) ;
#10183 = VECTOR ( 'NONE', #21164, 1000.000000000000000 ) ;
#10184 = VECTOR ( 'NONE', #9629, 1000.000000000000114 ) ;
#10185 = DIRECTION ( 'NONE',  ( -1.000000000000000000, -2.999999999999999839E-15, 0.000000000000000000 ) ) ;
#10186 = EDGE_CURVE ( 'NONE', #13333, #5803, #8338, .T. ) ;
#10187 = ORIENTED_EDGE ( 'NONE', *, *, #15205, .F. ) ;
#10188 = DIRECTION ( 'NONE',  ( 1.734723475976804876E-16, 2.999999999999999839E-15, 1.000000000000000000 ) ) ;
#10189 = DIRECTION ( 'NONE',  ( 0.000000000000000000, 1.000000000000000000, 0.000000000000000000 ) ) ;
#10190 = CARTESIAN_POINT ( 'NONE',  ( 37.50301148336529877, -2.503840866421917166, 73.69843995877330656 ) ) ;
#10191 = EDGE_CURVE ( 'NONE', #10854, #13157, #2514, .T. ) ;
#10192 = EDGE_CURVE ( 'NONE', #7024, #5182, #6147, .T. ) ;
#10193 = EDGE_CURVE ( 'NONE', #3194, #14256, #8780, .T. ) ;
#10194 = LINE ( 'NONE', #24327, #4539 ) ;
#10195 = FACE_OUTER_BOUND ( 'NONE', #13856, .T. ) ;
#10196 = CARTESIAN_POINT ( 'NONE',  ( 39.95015449827720744, -10.61368208888610631, 70.79240656858107172 ) ) ;
#10197 = CARTESIAN_POINT ( 'NONE',  ( 33.31606138205700773, -3.566646240838321269, 18.16837712155798457 ) ) ;
#10198 = DIRECTION ( 'NONE',  ( -1.000000000000000000, 0.000000000000000000, 0.000000000000000000 ) ) ;
#10199 = FACE_OUTER_BOUND ( 'NONE', #13504, .T. ) ;
#10200 = EDGE_CURVE ( 'NONE', #10286, #20311, #24031, .T. ) ;
#10201 = DIRECTION ( 'NONE',  ( 0.000000000000000000, 0.7540134720837717852, 0.6568589528324746407 ) ) ;
#10202 = AXIS2_PLACEMENT_3D ( 'NONE', #4392, #18176, #19847 ) ;
#10203 = CONTEXT_DEPENDENT_SHAPE_REPRESENTATION ( #7002, #8295 ) ;
#10204 = CARTESIAN_POINT ( 'NONE',  ( 32.81606138205700773, -34.55876147765401640, 70.30501292737011454 ) ) ;
#10205 = CARTESIAN_POINT ( 'NONE',  ( 37.38336156205273397, -25.90384086642191264, 70.63227792289245599 ) ) ;
#10206 = CARTESIAN_POINT ( 'NONE',  ( 39.82603832034400426, -12.31368208888610560, 72.40698646996133903 ) ) ;
#10207 = AXIS2_PLACEMENT_3D ( 'NONE', #14341, #21817, #10108 ) ;
#10208 = VECTOR ( 'NONE', #11060, 1000.000000000000000 ) ;
#10209 = CARTESIAN_POINT ( 'NONE',  ( 33.31606138205700773, -29.06829118875199924, 75.80501292737000085 ) ) ;
#10210 = CARTESIAN_POINT ( 'NONE',  ( 37.25202387243754032, -12.40384086642191619, 72.75271321436731853 ) ) ;
#10211 = LINE ( 'NONE', #23972, #11839 ) ;
#10212 = CARTESIAN_POINT ( 'NONE',  ( 39.95015449827720744, -14.61368208888610454, 70.79240656858105751 ) ) ;
#10213 = VERTEX_POINT ( 'NONE', #15806 ) ;
#10214 = CARTESIAN_POINT ( 'NONE',  ( 40.55423172469004811, -14.41368208888610347, 72.05058123536544201 ) ) ;
#10215 = ORIENTED_EDGE ( 'NONE', *, *, #21070, .T. ) ;
#10216 = PLANE ( 'NONE',  #11119 ) ;
#10217 = DIRECTION ( 'NONE',  ( 0.000000000000000000, 0.000000000000000000, 1.000000000000000000 ) ) ;
#10218 = CARTESIAN_POINT ( 'NONE',  ( 37.21915885897815457, -16.20384086642190979, 71.67976084211552745 ) ) ;
#10219 = ORIENTED_EDGE ( 'NONE', *, *, #10364, .F. ) ;
#10220 = VERTEX_POINT ( 'NONE', #2390 ) ;
#10221 = FACE_OUTER_BOUND ( 'NONE', #23883, .T. ) ;
#10222 = CYLINDRICAL_SURFACE ( 'NONE', #15768, 2.000000000000001776 ) ;
#10223 = CARTESIAN_POINT ( 'NONE',  ( 40.26954217208372455, -24.90384086642191619, 72.86986841596730358 ) ) ;
#10224 = EDGE_CURVE ( 'NONE', #11138, #19881, #13501, .T. ) ;
#10225 = ADVANCED_FACE ( 'NONE', ( #21731 ), #6404, .F. ) ;
#10226 = AXIS2_PLACEMENT_3D ( 'NONE', #9618, #9244, #25296 ) ;
#10227 = PLANE ( 'NONE',  #19817 ) ;
#10228 = CARTESIAN_POINT ( 'NONE',  ( 37.33957961208646736, -25.81368208888610738, 72.81632618279320468 ) ) ;
#10229 = CARTESIAN_POINT ( 'NONE',  ( 32.81606138205700773, -32.95845724189726411, 59.23979596822106686 ) ) ;
#10230 = ORIENTED_EDGE ( 'NONE', *, *, #4462, .F. ) ;
#10231 = FACE_OUTER_BOUND ( 'NONE', #23991, .T. ) ;
#10232 = DIRECTION ( 'NONE',  ( 0.000000000000000000, -0.5706330172266907974, 0.8212051873014217795 ) ) ;
#10233 = EDGE_CURVE ( 'NONE', #20855, #14994, #8207, .T. ) ;
#10234 = CARTESIAN_POINT ( 'NONE',  ( 38.26194895904384907, -18.60384086642191548, 73.11602215082116629 ) ) ;
#10235 = PLANE ( 'NONE',  #25188 ) ;
#10236 = VECTOR ( 'NONE', #18999, 1000.000000000000000 ) ;
#10237 = ORIENTED_EDGE ( 'NONE', *, *, #15077, .F. ) ;
#10238 = CARTESIAN_POINT ( 'NONE',  ( 45.81606138205697931, -5.229446354160903532, -9.573232046949343044 ) ) ;
#10239 = LINE ( 'NONE', #6118, #16453 ) ;
#10240 = CARTESIAN_POINT ( 'NONE',  ( 38.93415946300896024, -29.50384086642191050, 69.66206559358660400 ) ) ;
#10241 = DIRECTION ( 'NONE',  ( 0.000000000000000000, 1.000000000000000000, 0.000000000000000000 ) ) ;
#10242 = VERTEX_POINT ( 'NONE', #23663 ) ;
#10243 = VECTOR ( 'NONE', #1565, 999.9999999999998863 ) ;
#10244 = EDGE_CURVE ( 'NONE', #14645, #2100, #12077, .T. ) ;
#10245 = DIRECTION ( 'NONE',  ( 1.000000000000000000, 1.000000000000000078E-15, 0.000000000000000000 ) ) ;
#10246 = VERTEX_POINT ( 'NONE', #6275 ) ;
#10247 = ORIENTED_EDGE ( 'NONE', *, *, #6762, .T. ) ;
#10248 = CARTESIAN_POINT ( 'NONE',  ( 41.06606138205702194, -5.022037326221700404, -5.474317061061731771 ) ) ;
#10249 = CARTESIAN_POINT ( 'NONE',  ( 45.81606138205700063, 35.12314894770293705, 81.17823623207323180 ) ) ;
#10250 = CARTESIAN_POINT ( 'NONE',  ( 39.51027997493896748, -4.513682088886101340, 71.32335560751961623 ) ) ;
#10251 = AXIS2_PLACEMENT_3D ( 'NONE', #7091, #13152, #3858 ) ;
#10252 = CARTESIAN_POINT ( 'NONE',  ( 38.73920764526925353, -2.113682088886101873, 72.49843995877331793 ) ) ;
#10253 = EDGE_LOOP ( 'NONE', ( #5035, #11003, #23694, #3643 ) ) ;
#10254 = ORIENTED_EDGE ( 'NONE', *, *, #21218, .T. ) ;
#10255 = DIRECTION ( 'NONE',  ( -1.000000000000000000, -2.168404344971005170E-16, 1.734723475976814737E-16 ) ) ;
#10256 = FACE_OUTER_BOUND ( 'NONE', #10786, .T. ) ;
#10257 = CARTESIAN_POINT ( 'NONE',  ( 35.81606138205700063, -24.05876147765399864, 75.30501292737008612 ) ) ;
#10258 = CARTESIAN_POINT ( 'NONE',  ( 36.87297107704149823, -13.90384086642190908, 70.26145752964252722 ) ) ;
#10259 = VECTOR ( 'NONE', #20726, 1000.000000000000000 ) ;
#10260 = SPHERICAL_SURFACE ( 'NONE', #3781, 1.100000000000000089 ) ;
#10261 = DIRECTION ( 'NONE',  ( 0.000000000000000000, -0.8212051873014252212, -0.5706330172266858014 ) ) ;
#10262 = EDGE_LOOP ( 'NONE', ( #24729, #688, #15533, #21804 ) ) ;
#10263 = ORIENTED_EDGE ( 'NONE', *, *, #6350, .T. ) ;
#10264 = ORIENTED_EDGE ( 'NONE', *, *, #2727, .F. ) ;
#10265 = AXIS2_PLACEMENT_3D ( 'NONE', #1155, #9047, #22812 ) ;
#10266 = SHAPE_REPRESENTATION ( 'Pusher Guide Rod', ( #2000 ), #15364 ) ;
#10267 = CARTESIAN_POINT ( 'NONE',  ( 39.81746892067405952, 41.43850569188389699, 79.87823623207322044 ) ) ;
#10268 = CARTESIAN_POINT ( 'NONE',  ( 39.75915168707250302, -6.713682088886100630, 70.26145752964255564 ) ) ;
#10269 = CARTESIAN_POINT ( 'NONE',  ( 41.06606138205702194, -20.30191568716147898, 23.22716926412510219 ) ) ;
#10270 = CARTESIAN_POINT ( 'NONE',  ( 31.01606138205699992, 36.92314894770294131, 81.37823623207324886 ) ) ;
#10271 = AXIS2_PLACEMENT_3D ( 'NONE', #1122, #5000, #859 ) ;
#10272 = DIRECTION ( 'NONE',  ( -1.000000000000000000, -3.243061817617045614E-15, -1.199556157213611407E-16 ) ) ;
#10273 = FACE_OUTER_BOUND ( 'NONE', #1670, .T. ) ;
#10274 = EDGE_CURVE ( 'NONE', #3043, #13140, #6019, .T. ) ;
#10275 = CIRCLE ( 'NONE', #13161, 1.249999999999995115 ) ;
#10276 = CARTESIAN_POINT ( 'NONE',  ( 40.64099152588522657, -9.607181138187000258, 83.02501292736999972 ) ) ;
#10277 = DIRECTION ( 'NONE',  ( -1.133678928659556219E-16, 0.4425581086832399147, -0.8967398287344627850 ) ) ;
#10278 = ADVANCED_FACE ( 'NONE', ( #78, #4089 ), #11961, .T. ) ;
#10279 = CIRCLE ( 'NONE', #13564, 1.000000000000000888 ) ;
#10280 = DIRECTION ( 'NONE',  ( -1.000000000000000000, 0.000000000000000000, 0.000000000000000000 ) ) ;
#10281 = ORIENTED_EDGE ( 'NONE', *, *, #758, .F. ) ;
#10282 = VERTEX_POINT ( 'NONE', #8971 ) ;
#10283 = DIRECTION ( 'NONE',  ( -1.000000000000000000, -1.185526135920242153E-16, -8.246758300215675884E-17 ) ) ;
#10284 = CARTESIAN_POINT ( 'NONE',  ( 40.55423172469004101, -5.203840866421914235, 70.70992431699450265 ) ) ;
#10285 = AXIS2_PLACEMENT_3D ( 'NONE', #15837, #7614, #21387 ) ;
#10286 = VERTEX_POINT ( 'NONE', #22485 ) ;
#10287 = DIRECTION ( 'NONE',  ( -1.000000000000000000, 6.018531076210110289E-31, 1.734723475976804876E-16 ) ) ;
#10288 = CARTESIAN_POINT ( 'NONE',  ( 39.38009889167650357, -8.213682088886105959, 72.75271321436733274 ) ) ;
#10289 = AXIS2_PLACEMENT_3D ( 'NONE', #22595, #4950, #12820 ) ;
#10290 = LINE ( 'NONE', #23925, #4237 ) ;
#10291 = ADVANCED_FACE ( 'NONE', ( #2760 ), #14756, .T. ) ;
#10292 = CARTESIAN_POINT ( 'NONE',  ( 36.36258059203031934, -15.71368208888610773, 72.86986841596736042 ) ) ;
#10293 = AXIS2_PLACEMENT_3D ( 'NONE', #11744, #15582, #21516 ) ;
#10294 = LINE ( 'NONE', #6547, #20145 ) ;
#10295 = CARTESIAN_POINT ( 'NONE',  ( 33.31606138205700773, -16.48551471403133206, 77.11349248448009064 ) ) ;
#10296 = CARTESIAN_POINT ( 'NONE',  ( 32.56606138205700773, 40.39281886181299797, 82.55501292736983032 ) ) ;
#10297 = FILL_AREA_STYLE ('',( #18884 ) ) ;
#10298 = DIRECTION ( 'NONE',  ( 1.000000000000000000, 0.000000000000000000, 0.000000000000000000 ) ) ;
#10299 = CARTESIAN_POINT ( 'NONE',  ( 33.31606138205700773, -11.22674583108233115, 81.40610939240433197 ) ) ;
#10300 = CARTESIAN_POINT ( 'NONE',  ( 30.81606138205700418, -36.30035594811090505, 74.91924054225879104 ) ) ;
#10301 = CARTESIAN_POINT ( 'NONE',  ( 37.69225076346193504, -25.81368208888610027, 72.33091598616823603 ) ) ;
#10302 = ORIENTED_EDGE ( 'NONE', *, *, #3983, .F. ) ;
#10303 = AXIS2_PLACEMENT_3D ( 'NONE', #2463, #275, #10340 ) ;
#10304 = CARTESIAN_POINT ( 'NONE',  ( 40.11656585159207822, -21.15771639874553500, 75.86402839307550039 ) ) ;
#10305 = DIRECTION ( 'NONE',  ( 1.000000000000000000, -9.027796614315171564E-31, -4.436993566807132493E-46 ) ) ;
#10306 = VERTEX_POINT ( 'NONE', #1218 ) ;
#10307 = EDGE_LOOP ( 'NONE', ( #8049, #4302, #18356, #18215 ) ) ;
#10308 = UNCERTAINTY_MEASURE_WITH_UNIT (LENGTH_MEASURE( 1.000000000000000082E-05 ), #13225, 'distance_accuracy_value', 'NONE');
#10309 = CIRCLE ( 'NONE', #4151, 1.750000000000001554 ) ;
#10310 = CARTESIAN_POINT ( 'NONE',  ( 39.02088643472237806, -20.70384086642192401, 73.73360434286898624 ) ) ;
#10311 = CARTESIAN_POINT ( 'NONE',  ( 39.95015449827720744, -24.61368208888610454, 70.79240656858104330 ) ) ;
#10312 = LINE ( 'NONE', #4136, #20179 ) ;
#10313 = CARTESIAN_POINT ( 'NONE',  ( 36.81606138205700063, -4.399276463885007260, 59.51717649063222382 ) ) ;
#10314 = VERTEX_POINT ( 'NONE', #12967 ) ;
#10315 = CARTESIAN_POINT ( 'NONE',  ( 39.80936209861184238, -5.840161863587774782, 82.78488652399678926 ) ) ;
#10316 = DIRECTION ( 'NONE',  ( 1.156482317317871478E-16, 0.4425581086832399702, -0.8967398287344626739 ) ) ;
#10317 = EDGE_CURVE ( 'NONE', #13201, #20166, #20312, .T. ) ;
#10318 = CARTESIAN_POINT ( 'NONE',  ( 36.29569395875881099, -6.303840866421917433, 72.77780686321129622 ) ) ;
#10319 = CARTESIAN_POINT ( 'NONE',  ( 30.81606138205700418, -0.6071811381869983704, 122.0250129273699997 ) ) ;
#10320 = PLANE ( 'NONE',  #23113 ) ;
#10321 = CARTESIAN_POINT ( 'NONE',  ( 37.80618814713140097, -5.913682088886107024, 73.13360434286904876 ) ) ;
#10322 = DIRECTION ( 'NONE',  ( -1.000000000000000000, 1.115179377413661005E-30, 3.717264591378870232E-16 ) ) ;
#10323 = AXIS2_PLACEMENT_3D ( 'NONE', #21779, #20094, #2560 ) ;
#10324 = CARTESIAN_POINT ( 'NONE',  ( 36.49096545463212493, -27.51368208888610312, 71.43714994484031422 ) ) ;
#10325 = AXIS2_PLACEMENT_3D ( 'NONE', #2366, #16152, #13985 ) ;
#10326 = LINE ( 'NONE', #23836, #18410 ) ;
#10327 = CARTESIAN_POINT ( 'NONE',  ( 43.11717982288782025, 3.481773294781324690, 6.342591232598341122 ) ) ;
#10328 = EDGE_CURVE ( 'NONE', #14345, #3268, #5887, .T. ) ;
#10329 = CARTESIAN_POINT ( 'NONE',  ( 38.73920764526923932, -23.50384086642191050, 70.26206559358661252 ) ) ;
#10330 = CARTESIAN_POINT ( 'NONE',  ( 40.14115730948191185, -14.51368208888610667, 71.32335560751960202 ) ) ;
#10331 = ADVANCED_FACE ( 'NONE', ( #22362 ), #10901, .F. ) ;
#10332 = DIRECTION ( 'NONE',  ( -1.000000000000000000, -1.734723475976804876E-16, 1.734723475976814737E-16 ) ) ;
#10333 = CARTESIAN_POINT ( 'NONE',  ( 39.75915168707251723, -12.90384086642191797, 72.49904802271738902 ) ) ;
#10334 = EDGE_CURVE ( 'NONE', #23981, #22885, #8589, .T. ) ;
#10335 = CARTESIAN_POINT ( 'NONE',  ( 32.81606138205700773, -33.00876147765401925, 70.30501292737011454 ) ) ;
#10336 = CARTESIAN_POINT ( 'NONE',  ( 38.82593461698262871, -8.913682088886101695, 69.62690120949091011 ) ) ;
#10337 = EDGE_LOOP ( 'NONE', ( #5643, #15344, #23634, #23219, #24288, #5858, #19251, #298 ) ) ;
#10338 = CARTESIAN_POINT ( 'NONE',  ( 37.61123632939165873, -15.91368208888610880, 73.73360434286898624 ) ) ;
#10339 = ORIENTED_EDGE ( 'NONE', *, *, #13272, .F. ) ;
#10340 = DIRECTION ( 'NONE',  ( 0.000000000000000000, -1.000000000000000000, 2.775557561562890957E-15 ) ) ;
#10341 = DIRECTION ( 'NONE',  ( 1.000000000000000000, -6.018531076210130433E-31, -1.734723475976804876E-16 ) ) ;
#10342 = CIRCLE ( 'NONE', #48, 0.4999999999999943379 ) ;
#10343 = CARTESIAN_POINT ( 'NONE',  ( 38.37017380507018771, -17.60384086642191193, 70.24448340153875847 ) ) ;
#10344 = ORIENTED_EDGE ( 'NONE', *, *, #24091, .T. ) ;
#10345 = ORIENTED_EDGE ( 'NONE', *, *, #10359, .F. ) ;
#10346 = PLANE ( 'NONE',  #22822 ) ;
#10347 = DIRECTION ( 'NONE',  ( 1.000000000000000000, 1.000000000000000078E-15, 0.000000000000000000 ) ) ;
#10348 = CARTESIAN_POINT ( 'NONE',  ( 40.33642880535521869, -23.30384086642191477, 69.98269868914866265 ) ) ;
#10349 = FILL_AREA_STYLE_COLOUR ( '', #17355 ) ;
#10350 = CARTESIAN_POINT ( 'NONE',  ( 38.82593461698262871, -28.91368208888610525, 69.62690120949091011 ) ) ;
#10351 = CARTESIAN_POINT ( 'NONE',  ( 32.56606138205700773, 29.91058581477919986, 95.51211970855651145 ) ) ;
#10352 = ORIENTED_EDGE ( 'NONE', *, *, #491, .T. ) ;
#10353 = EDGE_LOOP ( 'NONE', ( #4255, #1532, #9877, #23094 ) ) ;
#10354 = CARTESIAN_POINT ( 'NONE',  ( 40.64099152588522657, -0.6071811381869983704, 80.05501292737000085 ) ) ;
#10355 = CYLINDRICAL_SURFACE ( 'NONE', #7302, 0.7499999999999985567 ) ;
#10356 = CARTESIAN_POINT ( 'NONE',  ( 36.64852494920107517, -12.20384086642190979, 71.86517103874048473 ) ) ;
#10357 = CYLINDRICAL_SURFACE ( 'NONE', #2182, 0.2000000000000057288 ) ;
#10358 = EDGE_CURVE ( 'NONE', #6560, #15661, #12712, .T. ) ;
#10359 = EDGE_CURVE ( 'NONE', #21318, #9870, #8370, .T. ) ;
#10360 = CARTESIAN_POINT ( 'NONE',  ( 29.81606138205707168, -36.80651332587436286, 65.82119181171029254 ) ) ;
#10361 = VECTOR ( 'NONE', #9444, 1000.000000000000000 ) ;
#10362 = ADVANCED_FACE ( 'NONE', ( #12593 ), #7160, .F. ) ;
#10363 = FACE_OUTER_BOUND ( 'NONE', #3392, .T. ) ;
#10364 = EDGE_CURVE ( 'NONE', #11492, #24026, #10526, .T. ) ;
#10365 = CARTESIAN_POINT ( 'NONE',  ( 37.69796330110505522, -28.50384086642191406, 73.09843995877328382 ) ) ;
#10366 = ADVANCED_FACE ( 'NONE', ( #2644 ), #6779, .F. ) ;
#10367 = CARTESIAN_POINT ( 'NONE',  ( 42.06606138205700063, 47.04446929126260102, 81.37823623207319201 ) ) ;
#10368 = ORIENTED_EDGE ( 'NONE', *, *, #9264, .T. ) ;
#10369 = DIRECTION ( 'NONE',  ( 2.312964634635742267E-15, -0.8967398287344634511, -0.4425581086832385824 ) ) ;
#10370 = ORIENTED_EDGE ( 'NONE', *, *, #18072, .F. ) ;
#10371 = VERTEX_POINT ( 'NONE', #18373 ) ;
#10372 = PLANE ( 'NONE',  #5758 ) ;
#10373 = LINE ( 'NONE', #8573, #22386 ) ;
#10374 = CARTESIAN_POINT ( 'NONE',  ( 38.37017380507020192, -6.013682088886104005, 72.51602215082118619 ) ) ;
#10375 = CARTESIAN_POINT ( 'NONE',  ( 37.89291511884476904, -7.113682088886103649, 70.26206559358664094 ) ) ;
#10376 = ORIENTED_EDGE ( 'NONE', *, *, #13756, .T. ) ;
#10377 = VERTEX_POINT ( 'NONE', #14875 ) ;
#10378 = DIRECTION ( 'NONE',  ( -1.000000000000000000, -1.734723475976804876E-16, 1.734723475976814737E-16 ) ) ;
#10379 = LINE ( 'NONE', #8325, #21092 ) ;
#10380 = ORIENTED_EDGE ( 'NONE', *, *, #24319, .T. ) ;
#10381 = EDGE_CURVE ( 'NONE', #2880, #3879, #11672, .T. ) ;
#10382 = CARTESIAN_POINT ( 'NONE',  ( 36.31606138205700773, -19.28757846107944474, 24.56123906878952567 ) ) ;
#10383 = CIRCLE ( 'NONE', #19021, 1.000000000000000888 ) ;
#10384 = CARTESIAN_POINT ( 'NONE',  ( 36.68196826583682935, -10.00384086642191406, 70.79240656858108593 ) ) ;
#10385 = EDGE_CURVE ( 'NONE', #8842, #6883, #9190, .T. ) ;
#10386 = AXIS2_PLACEMENT_3D ( 'NONE', #8156, #15999, #18929 ) ;
#10387 = CARTESIAN_POINT ( 'NONE',  ( 3.816061382056966433, -4.589472609077318133, -6.350807634294847404 ) ) ;
#10388 = TOROIDAL_SURFACE ( 'NONE', #11624, 0.9023161253044896801, 0.2000000000000000111 ) ;
#10389 = CARTESIAN_POINT ( 'NONE',  ( 40.31606138205700773, -19.13113579875042092, 24.60350147050422720 ) ) ;
#10390 = VERTEX_POINT ( 'NONE', #3150 ) ;
#10391 = ORIENTED_EDGE ( 'NONE', *, *, #1906, .T. ) ;
#10392 = VERTEX_POINT ( 'NONE', #14505 ) ;
#10393 = CARTESIAN_POINT ( 'NONE',  ( 41.81606138205700063, -21.26162886970023536, 44.16441745890789150 ) ) ;
#10394 = CARTESIAN_POINT ( 'NONE',  ( 36.49096545463212493, -7.513682088886103116, 71.43714994484035685 ) ) ;
#10395 = EDGE_CURVE ( 'NONE', #12560, #17608, #18880, .T. ) ;
#10396 = AXIS2_PLACEMENT_3D ( 'NONE', #11859, #19310, #17388 ) ;
#10397 = CARTESIAN_POINT ( 'NONE',  ( 32.81606138205700773, 32.99511671078946762, 63.14259751872857152 ) ) ;
#10398 = LINE ( 'NONE', #329, #20293 ) ;
#10399 = CARTESIAN_POINT ( 'NONE',  ( 36.87297107704152666, -23.71368208888610951, 72.49904802271738902 ) ) ;
#10400 = CARTESIAN_POINT ( 'NONE',  ( 39.86436010876736447, -29.10876147765401711, 70.06288980751138240 ) ) ;
#10401 = AXIS2_PLACEMENT_3D ( 'NONE', #10144, #20183, #4474 ) ;
#10402 = CARTESIAN_POINT ( 'NONE',  ( 32.56606138205700773, -26.74044063519535186, 84.30501292737007191 ) ) ;
#10403 = DIRECTION ( 'NONE',  ( -1.000000000000000000, 0.000000000000000000, 0.000000000000000000 ) ) ;
#10404 = VECTOR ( 'NONE', #17350, 1000.000000000000000 ) ;
#10405 = CARTESIAN_POINT ( 'NONE',  ( 30.81606138205700418, 40.83281886181300280, 79.30501292736983032 ) ) ;
#10406 = ORIENTED_EDGE ( 'NONE', *, *, #15936, .T. ) ;
#10407 = EDGE_LOOP ( 'NONE', ( #6389, #63, #1839, #3680 ) ) ;
#10408 = CARTESIAN_POINT ( 'NONE',  ( 31.81606138205700418, -33.00876147765401925, 70.30501292737011454 ) ) ;
#10409 = CARTESIAN_POINT ( 'NONE',  ( 39.02088643472237806, -2.703840866421919120, 73.73360434286902887 ) ) ;
#10410 = CARTESIAN_POINT ( 'NONE',  ( 37.31647492878122563, -23.31368208888610383, 70.72433947564853440 ) ) ;
#10411 = ORIENTED_EDGE ( 'NONE', *, *, #4153, .T. ) ;
#10412 = AXIS2_PLACEMENT_3D ( 'NONE', #22261, #24058, #6548 ) ;
#10413 = ORIENTED_EDGE ( 'NONE', *, *, #12874, .F. ) ;
#10414 = LINE ( 'NONE', #2782, #18194 ) ;
#10415 = CARTESIAN_POINT ( 'NONE',  ( 36.87297107704152666, -9.713682088886107735, 72.49904802271743165 ) ) ;
#10416 = CIRCLE ( 'NONE', #513, 0.7500000000000006661 ) ;
#10417 = DIRECTION ( 'NONE',  ( 1.000000000000000000, 1.734723475976804876E-16, -1.734723475976814737E-16 ) ) ;
#10418 = AXIS2_PLACEMENT_3D ( 'NONE', #4299, #4166, #10217 ) ;
#10419 = CARTESIAN_POINT ( 'NONE',  ( 36.07789103942398867, -13.41368208888610525, 70.70992431699450265 ) ) ;
#10420 = VECTOR ( 'NONE', #4973, 1000.000000000000000 ) ;
#10421 = ADVANCED_FACE ( 'NONE', ( #20556 ), #23559, .T. ) ;
#10422 = CARTESIAN_POINT ( 'NONE',  ( 36.06606138205695800, 0.3291273985901090882, 13.05748091128652533 ) ) ;
#10423 = EDGE_CURVE ( 'NONE', #19848, #6622, #2888, .T. ) ;
#10424 = CARTESIAN_POINT ( 'NONE',  ( 33.23058527440272059, 3.113468987225112006, 6.136968036621317069 ) ) ;
#10425 = PRODUCT_RELATED_PRODUCT_CATEGORY ( 'part', '', ( #9311 ) ) ;
#10426 = CARTESIAN_POINT ( 'NONE',  ( 39.60177068742361683, -28.78761913971833408, 70.01260438786866303 ) ) ;
#10427 = DIRECTION ( 'NONE',  ( -1.327674326049719602E-15, 0.4425581086832399147, -0.8967398287344627850 ) ) ;
#10428 = CIRCLE ( 'NONE', #24801, 1.000000000000000888 ) ;
#10429 = DIRECTION ( 'NONE',  ( -1.000000000000000000, 0.000000000000000000, 0.000000000000000000 ) ) ;
#10430 = FACE_OUTER_BOUND ( 'NONE', #2886, .T. ) ;
#10431 = CARTESIAN_POINT ( 'NONE',  ( 39.37952058850012804, -26.61368208888610809, 70.97781676520600058 ) ) ;
#10432 = EDGE_LOOP ( 'NONE', ( #19077, #3134, #16598, #3305 ) ) ;
#10433 = COLOUR_RGB ( '', 0.66274510, 0.83137255, 0.94901961) ;
#10434 = CARTESIAN_POINT ( 'NONE',  ( 39.32240756636089429, -21.95444950771180004, 75.30325578900897199 ) ) ;
#10435 = CARTESIAN_POINT ( 'NONE',  ( 32.31606138205700063, -20.93319939328399926, 43.78741072286599945 ) ) ;
#10436 = ORIENTED_EDGE ( 'NONE', *, *, #15933, .F. ) ;
#10437 = ORIENTED_EDGE ( 'NONE', *, *, #20498, .T. ) ;
#10438 = AXIS2_PLACEMENT_3D ( 'NONE', #12153, #9828, #16112 ) ;
#10439 = CARTESIAN_POINT ( 'NONE',  ( 39.02088643472237806, -24.70384086642192401, 73.73360434286898624 ) ) ;
#10440 = CIRCLE ( 'NONE', #12090, 10.49999999999999822 ) ;
#10441 = CARTESIAN_POINT ( 'NONE',  ( 36.64852494920107517, -27.41368208888610525, 70.89533451361945993 ) ) ;
#10442 = FACE_OUTER_BOUND ( 'NONE', #14376, .T. ) ;
#10443 = CARTESIAN_POINT ( 'NONE',  ( 43.81606138205700063, -33.36905983554797217, 58.95447945960771818 ) ) ;
#10444 = CARTESIAN_POINT ( 'NONE',  ( 32.81606138205700773, 28.12806996228107437, 66.30501292736992980 ) ) ;
#10445 = EDGE_LOOP ( 'NONE', ( #9528, #19486, #5620, #20818 ) ) ;
#10446 = AXIS2_PLACEMENT_3D ( 'NONE', #3656, #1849, #5476 ) ;
#10447 = FACE_BOUND ( 'NONE', #15819, .T. ) ;
#10448 = CARTESIAN_POINT ( 'NONE',  ( 31.81606138205700418, 40.39281886181299797, 80.75501292736983316 ) ) ;
#10449 = CARTESIAN_POINT ( 'NONE',  ( 36.98690846071097127, -1.803840866421911215, 69.45876917294177133 ) ) ;
#10450 = EDGE_CURVE ( 'NONE', #25135, #23863, #7543, .T. ) ;
#10451 = CARTESIAN_POINT ( 'NONE',  ( 38.37017380507020192, 1.986317911113890444, 73.11602215082119471 ) ) ;
#10453 = ADVANCED_FACE ( 'NONE', ( #25411 ), #22866, .F. ) ;
#10452 = DIRECTION ( 'NONE',  ( -0.000000000000000000, -3.469446951953613400E-15, -1.000000000000000000 ) ) ;
#10454 = PRESENTATION_LAYER_ASSIGNMENT (  '', '', ( #22379 ) ) ;
#10455 = CARTESIAN_POINT ( 'NONE',  ( 38.93415946300897446, -8.113682088886108090, 73.09843995877331224 ) ) ;
#10456 = CARTESIAN_POINT ( 'NONE',  ( 35.64099152588522657, -9.607181138187000258, 82.55501292736998664 ) ) ;
#10457 = VECTOR ( 'NONE', #9170, 1000.000000000000000 ) ;
#10458 = DIRECTION ( 'NONE',  ( -6.938893903907229955E-15, -1.000000000000000000, 3.000000000000000628E-15 ) ) ;
#10459 = VECTOR ( 'NONE', #20481, 1000.000000000000000 ) ;
#10460 = FACE_BOUND ( 'NONE', #21013, .T. ) ;
#10461 =( BOUNDED_SURFACE ( )  B_SPLINE_SURFACE ( 3, 2, ( 
 ( #15680, #23527, #13760, #9899, #3962, #11834, #2017, #82, #7967, #22585, #14723, #7257, #11129, #1061, #15105, #16663, #1322, #13062, #591, #8468, #5201, #2518, #7001, #4941, #20915, #5328, #3251, #12810, #11263, #20185, #24492, #22841, #22965, #10996, #10875, #9332, #9208, #6868, #16923, #5073, #18981, #15232, #23083, #12938, #18728, #20658, #2993, #17176, #17054, #14850, #24878, #20793, #21042, #10399, #16788, #13190, #12343, #18263, #3384, #8939, #25001, #24619, #22710, #19112, #3127, #18850, #1190, #9079, #1450, #24754, #7131, #7390, #14985, #17684, #11641, #21666, #15611, #19477, #17430, #1944, #11769, #17817, #3895, #1688, #21286, #9830, #23465, #15, #23598, #7898, #23332, #3629, #21549, #19603, #11514, #4019, #9581, #148, #15745, #5830, #13436, #25125, #25259, #5962, #9956, #13811, #25384, #5699, #7642, #7768, #1821, #17557, #11893, #19354, #15484, #19735, #8027, #5448, #13563, #2076, #15867, #21416, #3759, #13317, #15359, #9707, #21169, #7508, #3510, #13689, #11383, #23209, #19225, #1564, #9456, #17305, #5579, #6461, #21923, #18440, #4285, #10087, #8662, #14319, #4156, #10330, #24210, #8274, #16114, #22173, #20240, #22046, #23968, #6343, #2328, #771, #521, #12401, #12275, #18068, #12535, #14203, #2702, #8406, #16244, #10584, #4407, #10206, #24090, #20118, #8525, #14069, #14446, #2452, #19992, #23716, #6586, #16362, #2579, #18191, #4536, #10463, #18322, #641, #12024, #12155, #20371, #390, #6084, #22294, #13942, #4657, #21798, #19866, #2209, #17946, #264, #8142, #15987, #23841, #6212, #14567, #22678, #6709, #22926, #16889, #15072, #21008, #13156, #20878, #3350, #1418, #18950, #24720, #11226, #9045, #3216, #16493, #6969, #14952, #10842, #18564, #7094, #22424, #18693, #12782, #20493, #1289, #22809, #1027, #9172, #19076, #14820, #5287, #4775, #5034, #24586, #12905, #20759, #20625, #12654, #14688, #1152, #24337, #3092, #16624, #2828, #2957, #8911, #10719, #895, #8788, #17019, #24464, #16751, #6836, #5171, #4905, #10962, #18815, #13026, #11094, #24852, #7227, #22553, #23178, #17653, #21637, #9302, #1654, #23436, #20343, #13406, #19320, #15711, #19196, #9545, #21512, #11353, #5928, #3598, #21254, #25092, #11480, #24968, #17395, #3478, #21135, #1530, #9421, #3862, #7733, #5546, #11741, #13284, #5801, #9680, #23052, #5417, #1788, #7349, #25228, #17267, #17529, #1914, #25353, #7475, #7868, #17143, #15327, #19442 ),
 ( #11865, #19700, #7612, #15454, #23298, #5664, #13785, #15577, #13529, #13659, #21383, #23562, #15196, #3727, #19575, #11604, #9798, #3989, #17916, #4501, #11996, #23811, #8373, #13910, #10431, #19834, #14039, #12241, #2297, #10172, #2424, #6054, #10301, #19965, #24066, #16087, #18039, #15956, #20084, #4378, #20214, #22018, #234, #2175, #18164, #23937, #488, #16215, #6435, #21894, #10055, #14289, #22139, #8114, #12374, #6184, #2550, #2048, #14173, #4254, #21765, #12124, #9927, #17785, #113, #6312, #7997, #15835, #8242, #23689, #358, #4125, #7694, #5757, #15540, #3688, #5511, #23268, #9761, #4084, #23389, #25182, #21728, #11572, #1745, #2133, #23660, #7440, #17742, #15288, #25319, #15422, #25446, #13491, #11956, #19281, #15671, #13375, #23520, #2005, #21606, #7825, #5629, #19795, #21341, #11438, #10014, #5889, #21222, #11701, #75, #9642, #17494, #13750, #3952, #13621, #21473, #3818, #19407, #25054, #1876, #11826, #19540, #17614, #13872, #19665, #23139, #9888, #7958, #3559, #15803, #6016, #1618, #9512, #17356, #7574, #1481, #15658, #1609, #23507, #23256, #3676, #19528, #9630, #17730, #7431, #13478, #17600, #9373, #15279, #1990, #5615, #13858, #17346, #11559, #9872, #11426, #19781, #25170, #17481, #5876, #23378, #5745, #13736, #21209, #21594, #15526, #61, #1865, #13611, #21329, #3941, #11812, #21714, #7813, #19395, #7563, #19651, #9751, #7945, #15789, #23646, #1732, #15412, #25428, #6005, #25308, #4070, #7683, #11942, #17223, #25044, #21460, #3549, #23128, #5500, #3803, #13363, #19271, #11690, #9500, #8574, #12067, #12195, #14363, #4195, #24259, #21968, #14114, #17986, #4331, #17864, #20033, #21840, #13991, #19914, #2252, #22218, #566, #16037, #4583, #6131, #16283, #2500, #15908, #23764, #20164, #188, #2373, #10126, #10374, #20295, #18241, #311, #686, #10000, #8190, #12319, #12450, #439, #23889, #6629, #24130, #6253, #6387, #10250, #8447, #4706, #12581, #18117, #8320, #6506, #16159, #2629, #24010, #14243, #10507, #22088, #18360, #8067, #4451, #16410, #2119, #14489, #22347, #8836, #24888, #2873, #22597, #13074, #22470, #5339, #10763, #20670, #9091, #8953, #16798, #24764, #6761, #7144, #1070, #11142, #5086, #24631, #6881, #16933, #1202, #7267, #18863, #16674, #18603, #14997, #12950, #22850, #20925, #5211, #12822, #945, #11007, #3266, #24507, #18993, #14736, #15118, #1334, #20802, #4953, #14614, #3004, #9221, #22975 ),
 ( #10885, #17069, #20411, #18738, #2744, #3137, #10633, #18484, #7012, #14860, #819, #22722, #8705, #16536, #24388, #4819, #12699, #20539, #25273, #25012, #17568, #11526, #23223, #3771, #5712, #5589, #19123, #19236, #9840, #9467, #28, #11782, #3398, #13447, #17317, #9342, #13575, #17446, #17188, #19614, #1957, #13331, #25396, #11278, #19366, #1462, #17697, #21428, #7909, #15756, #23612, #7782, #13205, #21055, #15625, #11655, #7402, #19493, #23477, #15247, #3640, #1834, #7526, #23099, #9717, #5461, #15373, #25138, #21182, #5841, #13702, #21298, #21561, #3520, #1700, #11395, #1574, #9596, #7653, #15494, #23346, #3909, #11905, #4168, #16128, #10478, #14082, #6096, #2593, #10099, #8157, #8542, #4550, #13824, #24102, #21681, #6225, #21809, #6359, #19880, #18333, #160, #22056, #19746, #4420, #8418, #2466, #14216, #12036, #657, #2221, #17829, #16375, #12287, #2090, #18082, #6475, #16000, #23851, #20130, #10343, #4300, #21936, #12166, #17957, #5973, #8287, #18205, #20002, #277, #533, #2342, #22185, #23980, #10218, #403, #16257, #14332, #4032, #12416, #20255, #9970, #8038, #15878, #23731, #13952, #20773, #16640, #22438, #14832, #5047, #4788, #14964, #20509, #11108, #3103, #24599, #6725, #18453, #2841, #10976, #3229, #7109, #18705, #24474, #910, #1041, #4920, #10856, #18828, #12667, #10729, #22823, #18962, #24223, #6847, #12919, #5184, #18575, #8800, #13037, #8675, #14703, #1166, #783, #20894, #22565, #12792, #14580, #20636, #14458, #2971, #16506, #10602, #24350, #8921, #9059, #22690, #16765, #16901, #2714, #24733, #6982, #12548, #20384, #1301, #22312, #9187, #6599, #4670, #9692, #25241, #19092, #15591, #24863, #13169, #1666, #11617, #15342, #15212, #13671, #5679, #3365, #21267, #9435, #23313, #19588, #1927, #17281, #23064, #13542, #9315, #21398, #5430, #11366, #9561, #25105, #25365, #15086, #21149, #7624, #17033, #22940, #17542, #13298, #21526, #24983, #19208, #7750, #1432, #7240, #7362, #7488, #3740, #5559, #13419, #19458, #11242, #1800, #3492, #23449, #1545, #3874, #5815, #17408, #23191, #17157, #3611, #11753, #5305, #21023, #11494, #19334, #15466, #12490, #16319, #22256, #6666, #8010, #23701, #18520, #22509, #9812, #2188, #24298, #851, #13925, #19846, #16578, #19714, #10068, #22385, #11879, #6800, #4138, #21780, #129, #12007, #25488, #17927, #4003, #21650, #2061, #9939, #4741, #8611, #6065, #12614, #13796, #14528, #10547 ),
 ( #17798, #8742, #17668, #5940, #20333, #20453, #8485, #15846, #14649, #2784, #608, #14401, #24167, #16449, #12736, #20579, #6542, #4616, #10674, #2665, #24427, #18396, #727, #4862, #7880, #15727, #23577, #7050, #11184, #2912, #8873, #21095, #16843, #7437, #10926, #5129, #3440, #4992, #13371, #18774, #3177, #17107, #16973, #24806, #7309, #14778, #15160, #9129, #19157, #13116, #7186, #14902, #24924, #9261, #15285, #1375, #24678, #1110, #23013, #20967, #5378, #11317, #13245, #20839, #8995, #19033, #18646, #12990, #22636, #12858, #20712, #3047, #1494, #9380, #22762, #17229, #6926, #25052, #3308, #16711, #24544, #23135, #985, #11047, #18904, #5507, #10795, #1248, #15033, #22888, #5250, #17353, #5884, #15798, #19537, #19405, #17872, #9882, #7571, #25439, #13618, #1999, #23774, #6138, #21468, #1741, #17738, #13488, #70, #9639, #15536, #13747, #3814, #4079, #19278, #25316, #3949, #21217, #1616, #13866, #17491, #196, #3685, #23385, #21725, #23264, #3556, #11567, #11699, #7954, #9759, #17610, #23656, #15420, #6013, #1874, #11951, #21602, #7821, #7690, #19790, #2127, #8077, #19661, #5754, #15667, #10010, #11821, #15916, #11436, #9509, #23515, #25178, #5625, #21338, #12202, #4713, #10258, #825, #10514, #14371, #21975, #8199, #18124, #18367, #18494, #22355, #8456, #6395, #16167, #16291, #20172, #573, #694, #20041, #2384, #12588, #8712, #13999, #14252, #2636, #20419, #448, #24020, #2751, #23897, #22096, #8584, #16047, #10643, #8328, #4461, #4340, #12330, #2508, #4205, #10384, #6262, #320, #14125, #18249, #16419, #12459, #24139, #24267, #17995, #6637, #22228, #2260, #10134, #6514, #12075, #4590, #20304, #14497, #16544, #24396, #21847, #19922, #14623, #2882, #16940, #1341, #5095, #4962, #3405, #20934, #18611, #11016, #24640, #13080, #9348, #17195, #7020, #12831, #3275, #24516, #11148, #20677, #1079, #24771, #14868, #15126, #4826, #10893, #15004, #6770, #12707, #24895, #3013, #11286, #14744, #8962, #7274, #8843, #22478, #22605, #22729, #19000, #20811, #3145, #9229, #954, #17077, #12958, #22982, #7153, #18872, #18746, #5348, #13213, #19129, #5218, #16807, #1209, #21062, #22857, #1470, #20548, #10770, #9097, #16683, #6889, #5848, #23230, #15763, #21306, #11913, #21568, #25402, #7535, #19243, #3647, #3916, #4038, #7914, #19503, #17455, #1707, #1842, #5719, #11662, #11789, #5595, #13453, #23622, #19753, #25021, #25280, #13710, #5980 ),
 ( #11534, #15381, #2096, #15500, #13832, #15256, #23352, #7659, #13582, #21434, #19374, #5468, #9605, #9723, #9976, #3778, #25147, #21687, #17575, #7787, #7410, #23105, #13338, #17705, #21189, #15635, #23483, #19620, #1963, #3527, #1581, #9848, #11403, #36, #9475, #17323, #539, #16007, #12554, #23857, #4174, #2719, #8424, #23738, #4425, #18338, #2348, #10223, #16262, #14337, #16133, #18090, #410, #21941, #20389, #20136, #6480, #6364, #12171, #6604, #8292, #22319, #2474, #10348, #4677, #23985, #4307, #18210, #14222, #2598, #8164, #8547, #22061, #17835, #24107, #12293, #12041, #22192, #4555, #12423, #20262, #10484, #662, #6102, #6230, #14463, #14087, #166, #16380, #8044, #24229, #20007, #13958, #15883, #21814, #19887, #2227, #10104, #17963, #282, #8680, #16770, #790, #17039, #10982, #9193, #15093, #7245, #14970, #22947, #21029, #13044, #18834, #5312, #3110, #22828, #10607, #1048, #9065, #4926, #12672, #1172, #16513, #12798, #6852, #14586, #20900, #16909, #20641, #3235, #13176, #18458, #10862, #16647, #24739, #2846, #7115, #24480, #2977, #20779, #18712, #18968, #24357, #14708, #5189, #6733, #22443, #11114, #22570, #4793, #18580, #8927, #1307, #20514, #10735, #917, #24605, #24868, #6988, #14838, #8807, #22696, #5053, #12924, #19593, #13548, #17416, #15347, #25374, #9697, #15734, #1806, #25112, #19214, #7755, #21403, #15597, #21534, #23453, #21274, #1550, #19465, #17547, #9441, #1934, #7495, #23583, #5820, #3745, #11371, #23070, #23196, #13677, #7885, #11759, #23320, #3616, #5565, #5685, #9568, #15472, #3882, #17288, #13424, #9819, #5947, #3371, #11500, #17673, #5, #19340, #1673, #13801, #13304, #25247, #11249, #5436, #19098, #7630, #11625, #1437, #9320, #17164, #24989, #21155, #15218, #3497, #7370, #16235, #20102, #10074, #24080, #135, #10318, #22035, #9944, #17804, #14189, #11883, #15973, #23706, #4396, #14308, #12258, #6073, #20229, #4010, #8015, #6329, #6451, #19982, #19852, #18311, #18181, #15853, #376, #14056, #2441, #21656, #2065, #22155, #17932, #632, #4145, #23828, #4520, #13930, #6570, #12012, #21909, #505, #10190, #18053, #8393, #21786, #12389, #2312, #2568, #10449, #8260, #8130, #8514, #16351, #24199, #19721, #249, #2195, #6201, #4272, #12142, #16101, #23955, #6826, #12640, #5022, #20743, #20482, #5155, #10708, #1279, #10950, #14808, #22413, #8646, #18553, #18802, #18937, #22796, #8900, #14672, #16609 ),
 ( #22542, #3079, #13014, #877, #24454, #20864, #24323, #4891, #1141, #16476, #11082, #8773, #12770, #4763, #20614, #4645, #2944, #6695, #759, #14556, #2816, #9028, #12893, #10825, #16877, #18429, #24708, #22667, #2692, #10572, #6956, #12523, #18679, #1015, #7080, #14938, #3206, #16740, #9158, #22282, #24573, #17006, #24839, #14432, #20359, #3848, #21367, #19065, #11468, #25080, #13520, #9786, #17644, #7466, #13269, #3711, #24952, #11594, #21125, #1519, #17383, #15315, #15566, #5277, #11344, #15443, #19428, #1407, #19305, #23164, #1777, #7216, #15058, #5537, #3469, #9669, #7338, #17517, #19187, #9407, #25214, #13399, #23421, #13144, #17255, #23291, #22914, #20998, #25342, #21246, #11730, #15184, #3585, #7722, #9291, #3337, #23042, #1642, #5786, #9536, #7600, #13645, #17133, #21499, #5652, #19564, #1899, #11214, #5407, #22011, #6300, #12363, #23927, #21753, #15826, #4365, #10162, #12227, #18153, #20073, #17903, #23681, #16076, #14162, #6043, #16203, #4115, #20205, #2414, #349, #7986, #19691, #11986, #10292, #4493, #8363, #19952, #226, #2164, #2286, #6169, #12113, #476, #13897, #19824, #24056, #2537, #25475, #8103, #6427, #14276, #10041, #15947, #22127, #9917, #23801, #10419, #2036, #7857, #14030, #21884, #4243, #18028, #15698, #8231, #17773, #11851, #99, #23546, #5917, #13776, #21630, #3977, #22259, #6929, #18650, #6545, #14405, #10797, #8490, #12617, #20337, #990, #10928, #8876, #2668, #16847, #610, #4619, #2915, #12860, #16581, #16452, #14905, #8997, #16713, #6802, #4743, #14781, #24546, #5134, #22641, #14532, #8613, #4995, #20714, #3052, #18777, #1112, #10678, #24300, #24681, #7055, #6668, #22764, #22389, #12992, #20841, #3179, #730, #12493, #20455, #18285, #16322, #24169, #12742, #18523, #2789, #20582, #24431, #4864, #10549, #854, #8744, #18401, #14651, #22512, #3780, #38, #19756, #15502, #21438, #17838, #20970, #11665, #23625, #13118, #8046, #5722, #23356, #1380, #13585, #1252, #19505, #5252, #22890, #3311, #11188, #5982, #9850, #24926, #13834, #15035, #7916, #11791, #24810, #7190, #3918, #9132, #1844, #19036, #19622, #4041, #1968, #9265, #9978, #18907, #17109, #21570, #21689, #9724, #7311, #15885, #15767, #17578, #15638, #25407, #17708, #13961, #21816, #7790, #23484, #11916, #5852, #2097, #13713, #167, #23740, #6105, #11049, #16978, #8294, #12425, #4176, #10106, #22321, #18092, #8682, #12173, #6366, #4680 ),
 ( #16383, #10350, #12296, #18212, #20141, #16135, #17965, #2350, #14339, #16515, #2477, #4309, #793, #23988, #14224, #6737, #2721, #12043, #12556, #19890, #4427, #20010, #4560, #413, #24362, #23860, #20264, #286, #2601, #6607, #664, #10486, #10228, #14590, #22063, #16010, #2229, #18340, #8168, #16264, #20391, #542, #8426, #8549, #24231, #24109, #6482, #22194, #14467, #6232, #10609, #18460, #14089, #21944, #11252, #22699, #1440, #7119, #14974, #9323, #5058, #8929, #22830, #6990, #7247, #12800, #13179, #3116, #22446, #5192, #9069, #8813, #1310, #20782, #14841, #13050, #20903, #12927, #2850, #2980, #19102, #18718, #17167, #21033, #12675, #10986, #1051, #18583, #3239, #1177, #920, #3374, #24991, #22573, #9196, #20517, #18837, #10739, #7378, #11117, #4796, #16651, #24482, #17043, #6855, #14711, #24870, #18972, #4930, #15095, #22953, #20644, #16913, #5316, #16773, #10866, #24609, #24742, #9571, #11503, #19216, #7, #21540, #17419, #7888, #2068, #5688, #4013, #5439, #13552, #1553, #25116, #17294, #9821, #13680, #3619, #17676, #9446, #3886, #15601, #3500, #11374, #7758, #13307, #25250, #7498, #23456, #15736, #5822, #15350, #13804, #23074, #23200, #25376, #23587, #21406, #13427, #11887, #11762, #5568, #19467, #7633, #19596, #17807, #139, #15475, #21277, #1937, #19342, #5953, #1679, #23322, #21659, #3749, #19725, #21159, #11630, #9948, #15220, #1811, #9700, #17550, #12527, #15975, #10196, #635, #10078, #18432, #23832, #8263, #22160, #22038, #4399, #12392, #19855, #20233, #14193, #24201, #18184, #12262, #19985, #4526, #14311, #20365, #6454, #4275, #6203, #2570, #510, #10455, #8518, #18314, #380, #14059, #24083, #16354, #21912, #6574, #12146, #2695, #14437, #8396, #2316, #2198, #18057, #22286, #10578, #4648, #2445, #16106, #23958, #10321, #20109, #16238, #8019, #6333, #15858, #23709, #6076, #13934, #21790, #4147, #12016, #17936, #255, #8133, #10711, #10830, #13018, #2820, #22919, #20618, #12774, #16614, #2949, #16481, #18684, #20486, #4896, #9035, #762, #6699, #18943, #14681, #5280, #8778, #1020, #1282, #18557, #11218, #24458, #8904, #14943, #14812, #22671, #5160, #12647, #20871, #6961, #17010, #10955, #5027, #16745, #22800, #7086, #13148, #24712, #22546, #6830, #3210, #18809, #11087, #9164, #24845, #24580, #12897, #16880, #7220, #20747, #15062, #3085, #21000, #3342, #1145, #8652, #884, #24329, #14560, #22418, #4769, #17387 ) ),
 .UNSPECIFIED., .T., .F., .F. ) 
 B_SPLINE_SURFACE_WITH_KNOTS ( ( 4, 3, 4 ),
 ( 3, 2, 2, 2, 2, 2, 2, 2, 2, 2, 2, 2, 2, 2, 2, 2, 2, 2, 2, 2, 2, 2, 2, 2, 2, 2, 2, 2, 2, 2, 2, 2, 2, 2, 2, 2, 2, 2, 2, 2, 2, 2, 2, 2, 2, 2, 2, 2, 2, 2, 2, 2, 2, 2, 2, 2, 2, 2, 2, 2, 2, 2, 2, 2, 2, 2, 2, 2, 2, 2, 2, 2, 2, 2, 2, 2, 2, 2, 2, 2, 2, 2, 2, 2, 2, 2, 2, 2, 2, 2, 2, 2, 2, 2, 2, 2, 2, 2, 2, 2, 2, 2, 2, 2, 2, 2, 2, 2, 2, 2, 2, 2, 2, 2, 2, 2, 2, 2, 2, 2, 2, 2, 2, 2, 2, 2, 2, 2, 2, 2, 2, 2, 2, 2, 2, 2, 2, 2, 2, 2, 2, 2, 2, 2, 2, 2, 2, 2, 2, 2, 2, 2, 2, 2, 2, 3 ),
 ( 0.000000000000000000, 0.5000000000000000000, 1.000000000000000000 ),
 ( 0.000000000000000000, 0.006250000000000000347, 0.01250000000000000069, 0.01874999999999999931, 0.02500000000000000139, 0.03125000000000000000, 0.03749999999999999861, 0.04374999999999999722, 0.05000000000000000278, 0.05625000000000000139, 0.06250000000000000000, 0.06875000000000000555, 0.07499999999999999722, 0.08125000000000000278, 0.08749999999999999445, 0.09375000000000000000, 0.1000000000000000056, 0.1062499999999999972, 0.1125000000000000028, 0.1187499999999999944, 0.1250000000000000000, 0.1312500000000000056, 0.1375000000000000111, 0.1437499999999999889, 0.1499999999999999944, 0.1562500000000000000, 0.1625000000000000056, 0.1687500000000000111, 0.1749999999999999889, 0.1812499999999999944, 0.1875000000000000000, 0.1937500000000000056, 0.2000000000000000111, 0.2062499999999999889, 0.2124999999999999944, 0.2187500000000000000, 0.2250000000000000056, 0.2312500000000000111, 0.2374999999999999889, 0.2437499999999999944, 0.2500000000000000000, 0.2562499999999999778, 0.2625000000000000111, 0.2687499999999999889, 0.2750000000000000222, 0.2812500000000000000, 0.2874999999999999778, 0.2937500000000000111, 0.2999999999999999889, 0.3062500000000000222, 0.3125000000000000000, 0.3187499999999999778, 0.3250000000000000111, 0.3312499999999999889, 0.3375000000000000222, 0.3437500000000000000, 0.3499999999999999778, 0.3562500000000000111, 0.3624999999999999889, 0.3687500000000000222, 0.3750000000000000000, 0.3812499999999999778, 0.3875000000000000111, 0.3937499999999999889, 0.4000000000000000222, 0.4062500000000000000, 0.4124999999999999778, 0.4187500000000000111, 0.4249999999999999889, 0.4312500000000000222, 0.4375000000000000000, 0.4437499999999999778, 0.4500000000000000111, 0.4562499999999999889, 0.4625000000000000222, 0.4687500000000000000, 0.4749999999999999778, 0.4812500000000000111, 0.4874999999999999889, 0.4937500000000000222, 0.5000000000000000000, 0.5062499999999999778, 0.5124999999999999556, 0.5187500000000000444, 0.5250000000000000222, 0.5312500000000000000, 0.5374999999999999778, 0.5437499999999999556, 0.5500000000000000444, 0.5562500000000000222, 0.5625000000000000000, 0.5687499999999999778, 0.5749999999999999556, 0.5812500000000000444, 0.5875000000000000222, 0.5937500000000000000, 0.5999999999999999778, 0.6062499999999999556, 0.6125000000000000444, 0.6187500000000000222, 0.6250000000000000000, 0.6312499999999999778, 0.6374999999999999556, 0.6437500000000000444, 0.6500000000000000222, 0.6562500000000000000, 0.6624999999999999778, 0.6687499999999999556, 0.6750000000000000444, 0.6812500000000000222, 0.6875000000000000000, 0.6937499999999999778, 0.6999999999999999556, 0.7062500000000000444, 0.7125000000000000222, 0.7187500000000000000, 0.7249999999999999778, 0.7312499999999999556, 0.7375000000000000444, 0.7437500000000000222, 0.7500000000000000000, 0.7562499999999999778, 0.7624999999999999556, 0.7687500000000000444, 0.7750000000000000222, 0.7812500000000000000, 0.7874999999999999778, 0.7937499999999999556, 0.8000000000000000444, 0.8062500000000000222, 0.8125000000000000000, 0.8187499999999999778, 0.8249999999999999556, 0.8312500000000000444, 0.8375000000000000222, 0.8437500000000000000, 0.8499999999999999778, 0.8562499999999999556, 0.8625000000000000444, 0.8687500000000000222, 0.8750000000000000000, 0.8812499999999999778, 0.8874999999999999556, 0.8937500000000000444, 0.9000000000000000222, 0.9062500000000000000, 0.9124999999999999778, 0.9187499999999999556, 0.9250000000000000444, 0.9312500000000000222, 0.9375000000000000000, 0.9437499999999999778, 0.9499999999999999556, 0.9562500000000000444, 0.9625000000000000222, 0.9687500000000000000 ),
 .UNSPECIFIED. ) 
 GEOMETRIC_REPRESENTATION_ITEM ( )  RATIONAL_B_SPLINE_SURFACE ( (
 ( 1.000000000000000000, 0.9510565162951535312, 1.000000000000000000, 0.9510565162951535312, 1.000000000000000000, 0.9510565162951535312, 1.000000000000000000, 0.9510565162951535312, 1.000000000000000000, 0.9510565162951535312, 1.000000000000000000, 0.9510565162951535312, 1.000000000000000000, 0.9510565162951535312, 1.000000000000000000, 0.9510565162951535312, 1.000000000000000000, 0.9510565162951535312, 1.000000000000000000, 0.9510565162951535312, 1.000000000000000000, 0.9510565162951535312, 1.000000000000000000, 0.9510565162951535312, 1.000000000000000000, 0.9510565162951535312, 1.000000000000000000, 0.9510565162951535312, 1.000000000000000000, 0.9510565162951535312, 1.000000000000000000, 0.9510565162951535312, 1.000000000000000000, 0.9510565162951535312, 1.000000000000000000, 0.9510565162951535312, 1.000000000000000000, 0.9510565162951535312, 1.000000000000000000, 0.9510565162951535312, 1.000000000000000000, 0.9510565162951535312, 1.000000000000000000, 0.9510565162951535312, 1.000000000000000000, 0.9510565162951535312, 1.000000000000000000, 0.9510565162951535312, 1.000000000000000000, 0.9510565162951535312, 1.000000000000000000, 0.9510565162951535312, 1.000000000000000000, 0.9510565162951535312, 1.000000000000000000, 0.9510565162951535312, 1.000000000000000000, 0.9510565162951535312, 1.000000000000000000, 0.9510565162951535312, 1.000000000000000000, 0.9510565162951535312, 1.000000000000000000, 0.9510565162951535312, 1.000000000000000000, 0.9510565162951535312, 1.000000000000000000, 0.9510565162951535312, 1.000000000000000000, 0.9510565162951535312, 1.000000000000000000, 0.9510565162951535312, 1.000000000000000000, 0.9510565162951535312, 1.000000000000000000, 0.9510565162951535312, 1.000000000000000000, 0.9510565162951535312, 1.000000000000000000, 0.9510565162951535312, 1.000000000000000000, 0.9510565162951535312, 1.000000000000000000, 0.9510565162951535312, 1.000000000000000000, 0.9510565162951535312, 1.000000000000000000, 0.9510565162951535312, 1.000000000000000000, 0.9510565162951535312, 1.000000000000000000, 0.9510565162951535312, 1.000000000000000000, 0.9510565162951535312, 1.000000000000000000, 0.9510565162951535312, 1.000000000000000000, 0.9510565162951535312, 1.000000000000000000, 0.9510565162951535312, 1.000000000000000000, 0.9510565162951535312, 1.000000000000000000, 0.9510565162951535312, 1.000000000000000000, 0.9510565162951535312, 1.000000000000000000, 0.9510565162951535312, 1.000000000000000000, 0.9510565162951535312, 1.000000000000000000, 0.9510565162951535312, 1.000000000000000000, 0.9510565162951535312, 1.000000000000000000, 0.9510565162951535312, 1.000000000000000000, 0.9510565162951535312, 1.000000000000000000, 0.9510565162951535312, 1.000000000000000000, 0.9510565162951535312, 1.000000000000000000, 0.9510565162951535312, 1.000000000000000000, 0.9510565162951535312, 1.000000000000000000, 0.9510565162951535312, 1.000000000000000000, 0.9510565162951535312, 1.000000000000000000, 0.9510565162951535312, 1.000000000000000000, 0.9510565162951535312, 1.000000000000000000, 0.9510565162951535312, 1.000000000000000000, 0.9510565162951535312, 1.000000000000000000, 0.9510565162951535312, 1.000000000000000000, 0.9510565162951535312, 1.000000000000000000, 0.9510565162951535312, 1.000000000000000000, 0.9510565162951535312, 1.000000000000000000, 0.9510565162951535312, 1.000000000000000000, 0.9510565162951535312, 1.000000000000000000, 0.9510565162951535312, 1.000000000000000000, 0.9510565162951535312, 1.000000000000000000, 0.9510565162951535312, 1.000000000000000000, 0.9510565162951535312, 1.000000000000000000, 0.9510565162951535312, 1.000000000000000000, 0.9510565162951535312, 1.000000000000000000, 0.9510565162951535312, 1.000000000000000000, 0.9510565162951535312, 1.000000000000000000, 0.9510565162951535312, 1.000000000000000000, 0.9510565162951535312, 1.000000000000000000, 0.9510565162951535312, 1.000000000000000000, 0.9510565162951535312, 1.000000000000000000, 0.9510565162951535312, 1.000000000000000000, 0.9510565162951535312, 1.000000000000000000, 0.9510565162951535312, 1.000000000000000000, 0.9510565162951535312, 1.000000000000000000, 0.9510565162951535312, 1.000000000000000000, 0.9510565162951535312, 1.000000000000000000, 0.9510565162951535312, 1.000000000000000000, 0.9510565162951535312, 1.000000000000000000, 0.9510565162951535312, 1.000000000000000000, 0.9510565162951535312, 1.000000000000000000, 0.9510565162951535312, 1.000000000000000000, 0.9510565162951535312, 1.000000000000000000, 0.9510565162951535312, 1.000000000000000000, 0.9510565162951535312, 1.000000000000000000, 0.9510565162951535312, 1.000000000000000000, 0.9510565162951535312, 1.000000000000000000, 0.9510565162951535312, 1.000000000000000000, 0.9510565162951535312, 1.000000000000000000, 0.9510565162951535312, 1.000000000000000000, 0.9510565162951535312, 1.000000000000000000, 0.9510565162951535312, 1.000000000000000000, 0.9510565162951535312, 1.000000000000000000, 0.9510565162951535312, 1.000000000000000000, 0.9510565162951535312, 1.000000000000000000, 0.9510565162951535312, 1.000000000000000000, 0.9510565162951535312, 1.000000000000000000, 0.9510565162951535312, 1.000000000000000000, 0.9510565162951535312, 1.000000000000000000, 0.9510565162951535312, 1.000000000000000000, 0.9510565162951535312, 1.000000000000000000, 0.9510565162951535312, 1.000000000000000000, 0.9510565162951535312, 1.000000000000000000, 0.9510565162951535312, 1.000000000000000000, 0.9510565162951535312, 1.000000000000000000, 0.9510565162951535312, 1.000000000000000000, 0.9510565162951535312, 1.000000000000000000, 0.9510565162951535312, 1.000000000000000000, 0.9510565162951535312, 1.000000000000000000, 0.9510565162951535312, 1.000000000000000000, 0.9510565162951535312, 1.000000000000000000, 0.9510565162951535312, 1.000000000000000000, 0.9510565162951535312, 1.000000000000000000, 0.9510565162951535312, 1.000000000000000000, 0.9510565162951535312, 1.000000000000000000, 0.9510565162951535312, 1.000000000000000000, 0.9510565162951535312, 1.000000000000000000, 0.9510565162951535312, 1.000000000000000000, 0.9510565162951535312, 1.000000000000000000, 0.9510565162951535312, 1.000000000000000000, 0.9510565162951535312, 1.000000000000000000, 0.9510565162951535312, 1.000000000000000000, 0.9510565162951535312, 1.000000000000000000, 0.9510565162951535312, 1.000000000000000000, 0.9510565162951535312, 1.000000000000000000, 0.9510565162951535312, 1.000000000000000000, 0.9510565162951535312, 1.000000000000000000, 0.9510565162951535312, 1.000000000000000000, 0.9510565162951535312, 1.000000000000000000, 0.9510565162951535312, 1.000000000000000000, 0.9510565162951535312, 1.000000000000000000, 0.9510565162951535312, 1.000000000000000000, 0.9510565162951535312, 1.000000000000000000, 0.9510565162951535312, 1.000000000000000000, 0.9510565162951535312, 1.000000000000000000, 0.9510565162951535312, 1.000000000000000000, 0.9510565162951535312, 1.000000000000000000, 0.9510565162951535312, 1.000000000000000000, 0.9510565162951535312, 1.000000000000000000),
 ( 0.3333333333333333703, 0.3170188387650512141, 0.3333333333333333703, 0.3170188387650512141, 0.3333333333333333703, 0.3170188387650512141, 0.3333333333333333703, 0.3170188387650512141, 0.3333333333333333703, 0.3170188387650512141, 0.3333333333333333703, 0.3170188387650512141, 0.3333333333333333703, 0.3170188387650512141, 0.3333333333333333703, 0.3170188387650512141, 0.3333333333333333703, 0.3170188387650512141, 0.3333333333333333703, 0.3170188387650512141, 0.3333333333333333703, 0.3170188387650512141, 0.3333333333333333703, 0.3170188387650512141, 0.3333333333333333703, 0.3170188387650512141, 0.3333333333333333703, 0.3170188387650512141, 0.3333333333333333703, 0.3170188387650512141, 0.3333333333333333703, 0.3170188387650512141, 0.3333333333333333703, 0.3170188387650512141, 0.3333333333333333703, 0.3170188387650512141, 0.3333333333333333703, 0.3170188387650512141, 0.3333333333333333703, 0.3170188387650512141, 0.3333333333333333703, 0.3170188387650512141, 0.3333333333333333703, 0.3170188387650512141, 0.3333333333333333703, 0.3170188387650512141, 0.3333333333333333703, 0.3170188387650512141, 0.3333333333333333703, 0.3170188387650512141, 0.3333333333333333703, 0.3170188387650512141, 0.3333333333333333703, 0.3170188387650512141, 0.3333333333333333703, 0.3170188387650512141, 0.3333333333333333703, 0.3170188387650512141, 0.3333333333333333703, 0.3170188387650512141, 0.3333333333333333703, 0.3170188387650512141, 0.3333333333333333703, 0.3170188387650512141, 0.3333333333333333703, 0.3170188387650512141, 0.3333333333333333703, 0.3170188387650512141, 0.3333333333333333703, 0.3170188387650512141, 0.3333333333333333703, 0.3170188387650512141, 0.3333333333333333703, 0.3170188387650512141, 0.3333333333333333703, 0.3170188387650512141, 0.3333333333333333703, 0.3170188387650512141, 0.3333333333333333703, 0.3170188387650512141, 0.3333333333333333703, 0.3170188387650512141, 0.3333333333333333703, 0.3170188387650512141, 0.3333333333333333703, 0.3170188387650512141, 0.3333333333333333703, 0.3170188387650512141, 0.3333333333333333703, 0.3170188387650512141, 0.3333333333333333703, 0.3170188387650512141, 0.3333333333333333703, 0.3170188387650512141, 0.3333333333333333703, 0.3170188387650512141, 0.3333333333333333703, 0.3170188387650512141, 0.3333333333333333703, 0.3170188387650512141, 0.3333333333333333703, 0.3170188387650512141, 0.3333333333333333703, 0.3170188387650512141, 0.3333333333333333703, 0.3170188387650512141, 0.3333333333333333703, 0.3170188387650512141, 0.3333333333333333703, 0.3170188387650512141, 0.3333333333333333703, 0.3170188387650512141, 0.3333333333333333703, 0.3170188387650512141, 0.3333333333333333703, 0.3170188387650512141, 0.3333333333333333703, 0.3170188387650512141, 0.3333333333333333703, 0.3170188387650512141, 0.3333333333333333703, 0.3170188387650512141, 0.3333333333333333703, 0.3170188387650512141, 0.3333333333333333703, 0.3170188387650512141, 0.3333333333333333703, 0.3170188387650512141, 0.3333333333333333703, 0.3170188387650512141, 0.3333333333333333703, 0.3170188387650512141, 0.3333333333333333703, 0.3170188387650512141, 0.3333333333333333703, 0.3170188387650512141, 0.3333333333333333703, 0.3170188387650512141, 0.3333333333333333703, 0.3170188387650512141, 0.3333333333333333703, 0.3170188387650512141, 0.3333333333333333703, 0.3170188387650512141, 0.3333333333333333703, 0.3170188387650512141, 0.3333333333333333703, 0.3170188387650512141, 0.3333333333333333703, 0.3170188387650512141, 0.3333333333333333703, 0.3170188387650512141, 0.3333333333333333703, 0.3170188387650512141, 0.3333333333333333703, 0.3170188387650512141, 0.3333333333333333703, 0.3170188387650512141, 0.3333333333333333703, 0.3170188387650512141, 0.3333333333333333703, 0.3170188387650512141, 0.3333333333333333703, 0.3170188387650512141, 0.3333333333333333703, 0.3170188387650512141, 0.3333333333333333703, 0.3170188387650512141, 0.3333333333333333703, 0.3170188387650512141, 0.3333333333333333703, 0.3170188387650512141, 0.3333333333333333703, 0.3170188387650512141, 0.3333333333333333703, 0.3170188387650512141, 0.3333333333333333703, 0.3170188387650512141, 0.3333333333333333703, 0.3170188387650512141, 0.3333333333333333703, 0.3170188387650512141, 0.3333333333333333703, 0.3170188387650512141, 0.3333333333333333703, 0.3170188387650512141, 0.3333333333333333703, 0.3170188387650512141, 0.3333333333333333703, 0.3170188387650512141, 0.3333333333333333703, 0.3170188387650512141, 0.3333333333333333703, 0.3170188387650512141, 0.3333333333333333703, 0.3170188387650512141, 0.3333333333333333703, 0.3170188387650512141, 0.3333333333333333703, 0.3170188387650512141, 0.3333333333333333703, 0.3170188387650512141, 0.3333333333333333703, 0.3170188387650512141, 0.3333333333333333703, 0.3170188387650512141, 0.3333333333333333703, 0.3170188387650512141, 0.3333333333333333703, 0.3170188387650512141, 0.3333333333333333703, 0.3170188387650512141, 0.3333333333333333703, 0.3170188387650512141, 0.3333333333333333703, 0.3170188387650512141, 0.3333333333333333703, 0.3170188387650512141, 0.3333333333333333703, 0.3170188387650512141, 0.3333333333333333703, 0.3170188387650512141, 0.3333333333333333703, 0.3170188387650512141, 0.3333333333333333703, 0.3170188387650512141, 0.3333333333333333703, 0.3170188387650512141, 0.3333333333333333703, 0.3170188387650512141, 0.3333333333333333703, 0.3170188387650512141, 0.3333333333333333703, 0.3170188387650512141, 0.3333333333333333703, 0.3170188387650512141, 0.3333333333333333703, 0.3170188387650512141, 0.3333333333333333703, 0.3170188387650512141, 0.3333333333333333703, 0.3170188387650512141, 0.3333333333333333703, 0.3170188387650512141, 0.3333333333333333703, 0.3170188387650512141, 0.3333333333333333703, 0.3170188387650512141, 0.3333333333333333703, 0.3170188387650512141, 0.3333333333333333703, 0.3170188387650512141, 0.3333333333333333703, 0.3170188387650512141, 0.3333333333333333703, 0.3170188387650512141, 0.3333333333333333703, 0.3170188387650512141, 0.3333333333333333703, 0.3170188387650512141, 0.3333333333333333703, 0.3170188387650512141, 0.3333333333333333703, 0.3170188387650512141, 0.3333333333333333703, 0.3170188387650512141, 0.3333333333333333703, 0.3170188387650512141, 0.3333333333333333703, 0.3170188387650512141, 0.3333333333333333703, 0.3170188387650512141, 0.3333333333333333703, 0.3170188387650512141, 0.3333333333333333703, 0.3170188387650512141, 0.3333333333333333703, 0.3170188387650512141, 0.3333333333333333703, 0.3170188387650512141, 0.3333333333333333703, 0.3170188387650512141, 0.3333333333333333703, 0.3170188387650512141, 0.3333333333333333703, 0.3170188387650512141, 0.3333333333333333703, 0.3170188387650512141, 0.3333333333333333703, 0.3170188387650512141, 0.3333333333333333703, 0.3170188387650512141, 0.3333333333333333703, 0.3170188387650512141, 0.3333333333333333703, 0.3170188387650512141, 0.3333333333333333703, 0.3170188387650512141, 0.3333333333333333703, 0.3170188387650512141, 0.3333333333333333703, 0.3170188387650512141, 0.3333333333333333703, 0.3170188387650512141, 0.3333333333333333703, 0.3170188387650512141, 0.3333333333333333703, 0.3170188387650512141, 0.3333333333333333703, 0.3170188387650512141, 0.3333333333333333703),
 ( 0.3333333333333333703, 0.3170188387650512141, 0.3333333333333333703, 0.3170188387650512141, 0.3333333333333333703, 0.3170188387650512141, 0.3333333333333333703, 0.3170188387650512141, 0.3333333333333333703, 0.3170188387650512141, 0.3333333333333333703, 0.3170188387650512141, 0.3333333333333333703, 0.3170188387650512141, 0.3333333333333333703, 0.3170188387650512141, 0.3333333333333333703, 0.3170188387650512141, 0.3333333333333333703, 0.3170188387650512141, 0.3333333333333333703, 0.3170188387650512141, 0.3333333333333333703, 0.3170188387650512141, 0.3333333333333333703, 0.3170188387650512141, 0.3333333333333333703, 0.3170188387650512141, 0.3333333333333333703, 0.3170188387650512141, 0.3333333333333333703, 0.3170188387650512141, 0.3333333333333333703, 0.3170188387650512141, 0.3333333333333333703, 0.3170188387650512141, 0.3333333333333333703, 0.3170188387650512141, 0.3333333333333333703, 0.3170188387650512141, 0.3333333333333333703, 0.3170188387650512141, 0.3333333333333333703, 0.3170188387650512141, 0.3333333333333333703, 0.3170188387650512141, 0.3333333333333333703, 0.3170188387650512141, 0.3333333333333333703, 0.3170188387650512141, 0.3333333333333333703, 0.3170188387650512141, 0.3333333333333333703, 0.3170188387650512141, 0.3333333333333333703, 0.3170188387650512141, 0.3333333333333333703, 0.3170188387650512141, 0.3333333333333333703, 0.3170188387650512141, 0.3333333333333333703, 0.3170188387650512141, 0.3333333333333333703, 0.3170188387650512141, 0.3333333333333333703, 0.3170188387650512141, 0.3333333333333333703, 0.3170188387650512141, 0.3333333333333333703, 0.3170188387650512141, 0.3333333333333333703, 0.3170188387650512141, 0.3333333333333333703, 0.3170188387650512141, 0.3333333333333333703, 0.3170188387650512141, 0.3333333333333333703, 0.3170188387650512141, 0.3333333333333333703, 0.3170188387650512141, 0.3333333333333333703, 0.3170188387650512141, 0.3333333333333333703, 0.3170188387650512141, 0.3333333333333333703, 0.3170188387650512141, 0.3333333333333333703, 0.3170188387650512141, 0.3333333333333333703, 0.3170188387650512141, 0.3333333333333333703, 0.3170188387650512141, 0.3333333333333333703, 0.3170188387650512141, 0.3333333333333333703, 0.3170188387650512141, 0.3333333333333333703, 0.3170188387650512141, 0.3333333333333333703, 0.3170188387650512141, 0.3333333333333333703, 0.3170188387650512141, 0.3333333333333333703, 0.3170188387650512141, 0.3333333333333333703, 0.3170188387650512141, 0.3333333333333333703, 0.3170188387650512141, 0.3333333333333333703, 0.3170188387650512141, 0.3333333333333333703, 0.3170188387650512141, 0.3333333333333333703, 0.3170188387650512141, 0.3333333333333333703, 0.3170188387650512141, 0.3333333333333333703, 0.3170188387650512141, 0.3333333333333333703, 0.3170188387650512141, 0.3333333333333333703, 0.3170188387650512141, 0.3333333333333333703, 0.3170188387650512141, 0.3333333333333333703, 0.3170188387650512141, 0.3333333333333333703, 0.3170188387650512141, 0.3333333333333333703, 0.3170188387650512141, 0.3333333333333333703, 0.3170188387650512141, 0.3333333333333333703, 0.3170188387650512141, 0.3333333333333333703, 0.3170188387650512141, 0.3333333333333333703, 0.3170188387650512141, 0.3333333333333333703, 0.3170188387650512141, 0.3333333333333333703, 0.3170188387650512141, 0.3333333333333333703, 0.3170188387650512141, 0.3333333333333333703, 0.3170188387650512141, 0.3333333333333333703, 0.3170188387650512141, 0.3333333333333333703, 0.3170188387650512141, 0.3333333333333333703, 0.3170188387650512141, 0.3333333333333333703, 0.3170188387650512141, 0.3333333333333333703, 0.3170188387650512141, 0.3333333333333333703, 0.3170188387650512141, 0.3333333333333333703, 0.3170188387650512141, 0.3333333333333333703, 0.3170188387650512141, 0.3333333333333333703, 0.3170188387650512141, 0.3333333333333333703, 0.3170188387650512141, 0.3333333333333333703, 0.3170188387650512141, 0.3333333333333333703, 0.3170188387650512141, 0.3333333333333333703, 0.3170188387650512141, 0.3333333333333333703, 0.3170188387650512141, 0.3333333333333333703, 0.3170188387650512141, 0.3333333333333333703, 0.3170188387650512141, 0.3333333333333333703, 0.3170188387650512141, 0.3333333333333333703, 0.3170188387650512141, 0.3333333333333333703, 0.3170188387650512141, 0.3333333333333333703, 0.3170188387650512141, 0.3333333333333333703, 0.3170188387650512141, 0.3333333333333333703, 0.3170188387650512141, 0.3333333333333333703, 0.3170188387650512141, 0.3333333333333333703, 0.3170188387650512141, 0.3333333333333333703, 0.3170188387650512141, 0.3333333333333333703, 0.3170188387650512141, 0.3333333333333333703, 0.3170188387650512141, 0.3333333333333333703, 0.3170188387650512141, 0.3333333333333333703, 0.3170188387650512141, 0.3333333333333333703, 0.3170188387650512141, 0.3333333333333333703, 0.3170188387650512141, 0.3333333333333333703, 0.3170188387650512141, 0.3333333333333333703, 0.3170188387650512141, 0.3333333333333333703, 0.3170188387650512141, 0.3333333333333333703, 0.3170188387650512141, 0.3333333333333333703, 0.3170188387650512141, 0.3333333333333333703, 0.3170188387650512141, 0.3333333333333333703, 0.3170188387650512141, 0.3333333333333333703, 0.3170188387650512141, 0.3333333333333333703, 0.3170188387650512141, 0.3333333333333333703, 0.3170188387650512141, 0.3333333333333333703, 0.3170188387650512141, 0.3333333333333333703, 0.3170188387650512141, 0.3333333333333333703, 0.3170188387650512141, 0.3333333333333333703, 0.3170188387650512141, 0.3333333333333333703, 0.3170188387650512141, 0.3333333333333333703, 0.3170188387650512141, 0.3333333333333333703, 0.3170188387650512141, 0.3333333333333333703, 0.3170188387650512141, 0.3333333333333333703, 0.3170188387650512141, 0.3333333333333333703, 0.3170188387650512141, 0.3333333333333333703, 0.3170188387650512141, 0.3333333333333333703, 0.3170188387650512141, 0.3333333333333333703, 0.3170188387650512141, 0.3333333333333333703, 0.3170188387650512141, 0.3333333333333333703, 0.3170188387650512141, 0.3333333333333333703, 0.3170188387650512141, 0.3333333333333333703, 0.3170188387650512141, 0.3333333333333333703, 0.3170188387650512141, 0.3333333333333333703, 0.3170188387650512141, 0.3333333333333333703, 0.3170188387650512141, 0.3333333333333333703, 0.3170188387650512141, 0.3333333333333333703, 0.3170188387650512141, 0.3333333333333333703, 0.3170188387650512141, 0.3333333333333333703, 0.3170188387650512141, 0.3333333333333333703, 0.3170188387650512141, 0.3333333333333333703, 0.3170188387650512141, 0.3333333333333333703, 0.3170188387650512141, 0.3333333333333333703, 0.3170188387650512141, 0.3333333333333333703, 0.3170188387650512141, 0.3333333333333333703, 0.3170188387650512141, 0.3333333333333333703, 0.3170188387650512141, 0.3333333333333333703, 0.3170188387650512141, 0.3333333333333333703, 0.3170188387650512141, 0.3333333333333333703, 0.3170188387650512141, 0.3333333333333333703, 0.3170188387650512141, 0.3333333333333333703, 0.3170188387650512141, 0.3333333333333333703, 0.3170188387650512141, 0.3333333333333333703, 0.3170188387650512141, 0.3333333333333333703, 0.3170188387650512141, 0.3333333333333333703, 0.3170188387650512141, 0.3333333333333333703, 0.3170188387650512141, 0.3333333333333333703),
 ( 1.000000000000000000, 0.9510565162951535312, 1.000000000000000000, 0.9510565162951535312, 1.000000000000000000, 0.9510565162951535312, 1.000000000000000000, 0.9510565162951535312, 1.000000000000000000, 0.9510565162951535312, 1.000000000000000000, 0.9510565162951535312, 1.000000000000000000, 0.9510565162951535312, 1.000000000000000000, 0.9510565162951535312, 1.000000000000000000, 0.9510565162951535312, 1.000000000000000000, 0.9510565162951535312, 1.000000000000000000, 0.9510565162951535312, 1.000000000000000000, 0.9510565162951535312, 1.000000000000000000, 0.9510565162951535312, 1.000000000000000000, 0.9510565162951535312, 1.000000000000000000, 0.9510565162951535312, 1.000000000000000000, 0.9510565162951535312, 1.000000000000000000, 0.9510565162951535312, 1.000000000000000000, 0.9510565162951535312, 1.000000000000000000, 0.9510565162951535312, 1.000000000000000000, 0.9510565162951535312, 1.000000000000000000, 0.9510565162951535312, 1.000000000000000000, 0.9510565162951535312, 1.000000000000000000, 0.9510565162951535312, 1.000000000000000000, 0.9510565162951535312, 1.000000000000000000, 0.9510565162951535312, 1.000000000000000000, 0.9510565162951535312, 1.000000000000000000, 0.9510565162951535312, 1.000000000000000000, 0.9510565162951535312, 1.000000000000000000, 0.9510565162951535312, 1.000000000000000000, 0.9510565162951535312, 1.000000000000000000, 0.9510565162951535312, 1.000000000000000000, 0.9510565162951535312, 1.000000000000000000, 0.9510565162951535312, 1.000000000000000000, 0.9510565162951535312, 1.000000000000000000, 0.9510565162951535312, 1.000000000000000000, 0.9510565162951535312, 1.000000000000000000, 0.9510565162951535312, 1.000000000000000000, 0.9510565162951535312, 1.000000000000000000, 0.9510565162951535312, 1.000000000000000000, 0.9510565162951535312, 1.000000000000000000, 0.9510565162951535312, 1.000000000000000000, 0.9510565162951535312, 1.000000000000000000, 0.9510565162951535312, 1.000000000000000000, 0.9510565162951535312, 1.000000000000000000, 0.9510565162951535312, 1.000000000000000000, 0.9510565162951535312, 1.000000000000000000, 0.9510565162951535312, 1.000000000000000000, 0.9510565162951535312, 1.000000000000000000, 0.9510565162951535312, 1.000000000000000000, 0.9510565162951535312, 1.000000000000000000, 0.9510565162951535312, 1.000000000000000000, 0.9510565162951535312, 1.000000000000000000, 0.9510565162951535312, 1.000000000000000000, 0.9510565162951535312, 1.000000000000000000, 0.9510565162951535312, 1.000000000000000000, 0.9510565162951535312, 1.000000000000000000, 0.9510565162951535312, 1.000000000000000000, 0.9510565162951535312, 1.000000000000000000, 0.9510565162951535312, 1.000000000000000000, 0.9510565162951535312, 1.000000000000000000, 0.9510565162951535312, 1.000000000000000000, 0.9510565162951535312, 1.000000000000000000, 0.9510565162951535312, 1.000000000000000000, 0.9510565162951535312, 1.000000000000000000, 0.9510565162951535312, 1.000000000000000000, 0.9510565162951535312, 1.000000000000000000, 0.9510565162951535312, 1.000000000000000000, 0.9510565162951535312, 1.000000000000000000, 0.9510565162951535312, 1.000000000000000000, 0.9510565162951535312, 1.000000000000000000, 0.9510565162951535312, 1.000000000000000000, 0.9510565162951535312, 1.000000000000000000, 0.9510565162951535312, 1.000000000000000000, 0.9510565162951535312, 1.000000000000000000, 0.9510565162951535312, 1.000000000000000000, 0.9510565162951535312, 1.000000000000000000, 0.9510565162951535312, 1.000000000000000000, 0.9510565162951535312, 1.000000000000000000, 0.9510565162951535312, 1.000000000000000000, 0.9510565162951535312, 1.000000000000000000, 0.9510565162951535312, 1.000000000000000000, 0.9510565162951535312, 1.000000000000000000, 0.9510565162951535312, 1.000000000000000000, 0.9510565162951535312, 1.000000000000000000, 0.9510565162951535312, 1.000000000000000000, 0.9510565162951535312, 1.000000000000000000, 0.9510565162951535312, 1.000000000000000000, 0.9510565162951535312, 1.000000000000000000, 0.9510565162951535312, 1.000000000000000000, 0.9510565162951535312, 1.000000000000000000, 0.9510565162951535312, 1.000000000000000000, 0.9510565162951535312, 1.000000000000000000, 0.9510565162951535312, 1.000000000000000000, 0.9510565162951535312, 1.000000000000000000, 0.9510565162951535312, 1.000000000000000000, 0.9510565162951535312, 1.000000000000000000, 0.9510565162951535312, 1.000000000000000000, 0.9510565162951535312, 1.000000000000000000, 0.9510565162951535312, 1.000000000000000000, 0.9510565162951535312, 1.000000000000000000, 0.9510565162951535312, 1.000000000000000000, 0.9510565162951535312, 1.000000000000000000, 0.9510565162951535312, 1.000000000000000000, 0.9510565162951535312, 1.000000000000000000, 0.9510565162951535312, 1.000000000000000000, 0.9510565162951535312, 1.000000000000000000, 0.9510565162951535312, 1.000000000000000000, 0.9510565162951535312, 1.000000000000000000, 0.9510565162951535312, 1.000000000000000000, 0.9510565162951535312, 1.000000000000000000, 0.9510565162951535312, 1.000000000000000000, 0.9510565162951535312, 1.000000000000000000, 0.9510565162951535312, 1.000000000000000000, 0.9510565162951535312, 1.000000000000000000, 0.9510565162951535312, 1.000000000000000000, 0.9510565162951535312, 1.000000000000000000, 0.9510565162951535312, 1.000000000000000000, 0.9510565162951535312, 1.000000000000000000, 0.9510565162951535312, 1.000000000000000000, 0.9510565162951535312, 1.000000000000000000, 0.9510565162951535312, 1.000000000000000000, 0.9510565162951535312, 1.000000000000000000, 0.9510565162951535312, 1.000000000000000000, 0.9510565162951535312, 1.000000000000000000, 0.9510565162951535312, 1.000000000000000000, 0.9510565162951535312, 1.000000000000000000, 0.9510565162951535312, 1.000000000000000000, 0.9510565162951535312, 1.000000000000000000, 0.9510565162951535312, 1.000000000000000000, 0.9510565162951535312, 1.000000000000000000, 0.9510565162951535312, 1.000000000000000000, 0.9510565162951535312, 1.000000000000000000, 0.9510565162951535312, 1.000000000000000000, 0.9510565162951535312, 1.000000000000000000, 0.9510565162951535312, 1.000000000000000000, 0.9510565162951535312, 1.000000000000000000, 0.9510565162951535312, 1.000000000000000000, 0.9510565162951535312, 1.000000000000000000, 0.9510565162951535312, 1.000000000000000000, 0.9510565162951535312, 1.000000000000000000, 0.9510565162951535312, 1.000000000000000000, 0.9510565162951535312, 1.000000000000000000, 0.9510565162951535312, 1.000000000000000000, 0.9510565162951535312, 1.000000000000000000, 0.9510565162951535312, 1.000000000000000000, 0.9510565162951535312, 1.000000000000000000, 0.9510565162951535312, 1.000000000000000000, 0.9510565162951535312, 1.000000000000000000, 0.9510565162951535312, 1.000000000000000000, 0.9510565162951535312, 1.000000000000000000, 0.9510565162951535312, 1.000000000000000000, 0.9510565162951535312, 1.000000000000000000, 0.9510565162951535312, 1.000000000000000000, 0.9510565162951535312, 1.000000000000000000, 0.9510565162951535312, 1.000000000000000000),
 ( 0.3333333333333333703, 0.3170188387650512141, 0.3333333333333333703, 0.3170188387650512141, 0.3333333333333333703, 0.3170188387650512141, 0.3333333333333333703, 0.3170188387650512141, 0.3333333333333333703, 0.3170188387650512141, 0.3333333333333333703, 0.3170188387650512141, 0.3333333333333333703, 0.3170188387650512141, 0.3333333333333333703, 0.3170188387650512141, 0.3333333333333333703, 0.3170188387650512141, 0.3333333333333333703, 0.3170188387650512141, 0.3333333333333333703, 0.3170188387650512141, 0.3333333333333333703, 0.3170188387650512141, 0.3333333333333333703, 0.3170188387650512141, 0.3333333333333333703, 0.3170188387650512141, 0.3333333333333333703, 0.3170188387650512141, 0.3333333333333333703, 0.3170188387650512141, 0.3333333333333333703, 0.3170188387650512141, 0.3333333333333333703, 0.3170188387650512141, 0.3333333333333333703, 0.3170188387650512141, 0.3333333333333333703, 0.3170188387650512141, 0.3333333333333333703, 0.3170188387650512141, 0.3333333333333333703, 0.3170188387650512141, 0.3333333333333333703, 0.3170188387650512141, 0.3333333333333333703, 0.3170188387650512141, 0.3333333333333333703, 0.3170188387650512141, 0.3333333333333333703, 0.3170188387650512141, 0.3333333333333333703, 0.3170188387650512141, 0.3333333333333333703, 0.3170188387650512141, 0.3333333333333333703, 0.3170188387650512141, 0.3333333333333333703, 0.3170188387650512141, 0.3333333333333333703, 0.3170188387650512141, 0.3333333333333333703, 0.3170188387650512141, 0.3333333333333333703, 0.3170188387650512141, 0.3333333333333333703, 0.3170188387650512141, 0.3333333333333333703, 0.3170188387650512141, 0.3333333333333333703, 0.3170188387650512141, 0.3333333333333333703, 0.3170188387650512141, 0.3333333333333333703, 0.3170188387650512141, 0.3333333333333333703, 0.3170188387650512141, 0.3333333333333333703, 0.3170188387650512141, 0.3333333333333333703, 0.3170188387650512141, 0.3333333333333333703, 0.3170188387650512141, 0.3333333333333333703, 0.3170188387650512141, 0.3333333333333333703, 0.3170188387650512141, 0.3333333333333333703, 0.3170188387650512141, 0.3333333333333333703, 0.3170188387650512141, 0.3333333333333333703, 0.3170188387650512141, 0.3333333333333333703, 0.3170188387650512141, 0.3333333333333333703, 0.3170188387650512141, 0.3333333333333333703, 0.3170188387650512141, 0.3333333333333333703, 0.3170188387650512141, 0.3333333333333333703, 0.3170188387650512141, 0.3333333333333333703, 0.3170188387650512141, 0.3333333333333333703, 0.3170188387650512141, 0.3333333333333333703, 0.3170188387650512141, 0.3333333333333333703, 0.3170188387650512141, 0.3333333333333333703, 0.3170188387650512141, 0.3333333333333333703, 0.3170188387650512141, 0.3333333333333333703, 0.3170188387650512141, 0.3333333333333333703, 0.3170188387650512141, 0.3333333333333333703, 0.3170188387650512141, 0.3333333333333333703, 0.3170188387650512141, 0.3333333333333333703, 0.3170188387650512141, 0.3333333333333333703, 0.3170188387650512141, 0.3333333333333333703, 0.3170188387650512141, 0.3333333333333333703, 0.3170188387650512141, 0.3333333333333333703, 0.3170188387650512141, 0.3333333333333333703, 0.3170188387650512141, 0.3333333333333333703, 0.3170188387650512141, 0.3333333333333333703, 0.3170188387650512141, 0.3333333333333333703, 0.3170188387650512141, 0.3333333333333333703, 0.3170188387650512141, 0.3333333333333333703, 0.3170188387650512141, 0.3333333333333333703, 0.3170188387650512141, 0.3333333333333333703, 0.3170188387650512141, 0.3333333333333333703, 0.3170188387650512141, 0.3333333333333333703, 0.3170188387650512141, 0.3333333333333333703, 0.3170188387650512141, 0.3333333333333333703, 0.3170188387650512141, 0.3333333333333333703, 0.3170188387650512141, 0.3333333333333333703, 0.3170188387650512141, 0.3333333333333333703, 0.3170188387650512141, 0.3333333333333333703, 0.3170188387650512141, 0.3333333333333333703, 0.3170188387650512141, 0.3333333333333333703, 0.3170188387650512141, 0.3333333333333333703, 0.3170188387650512141, 0.3333333333333333703, 0.3170188387650512141, 0.3333333333333333703, 0.3170188387650512141, 0.3333333333333333703, 0.3170188387650512141, 0.3333333333333333703, 0.3170188387650512141, 0.3333333333333333703, 0.3170188387650512141, 0.3333333333333333703, 0.3170188387650512141, 0.3333333333333333703, 0.3170188387650512141, 0.3333333333333333703, 0.3170188387650512141, 0.3333333333333333703, 0.3170188387650512141, 0.3333333333333333703, 0.3170188387650512141, 0.3333333333333333703, 0.3170188387650512141, 0.3333333333333333703, 0.3170188387650512141, 0.3333333333333333703, 0.3170188387650512141, 0.3333333333333333703, 0.3170188387650512141, 0.3333333333333333703, 0.3170188387650512141, 0.3333333333333333703, 0.3170188387650512141, 0.3333333333333333703, 0.3170188387650512141, 0.3333333333333333703, 0.3170188387650512141, 0.3333333333333333703, 0.3170188387650512141, 0.3333333333333333703, 0.3170188387650512141, 0.3333333333333333703, 0.3170188387650512141, 0.3333333333333333703, 0.3170188387650512141, 0.3333333333333333703, 0.3170188387650512141, 0.3333333333333333703, 0.3170188387650512141, 0.3333333333333333703, 0.3170188387650512141, 0.3333333333333333703, 0.3170188387650512141, 0.3333333333333333703, 0.3170188387650512141, 0.3333333333333333703, 0.3170188387650512141, 0.3333333333333333703, 0.3170188387650512141, 0.3333333333333333703, 0.3170188387650512141, 0.3333333333333333703, 0.3170188387650512141, 0.3333333333333333703, 0.3170188387650512141, 0.3333333333333333703, 0.3170188387650512141, 0.3333333333333333703, 0.3170188387650512141, 0.3333333333333333703, 0.3170188387650512141, 0.3333333333333333703, 0.3170188387650512141, 0.3333333333333333703, 0.3170188387650512141, 0.3333333333333333703, 0.3170188387650512141, 0.3333333333333333703, 0.3170188387650512141, 0.3333333333333333703, 0.3170188387650512141, 0.3333333333333333703, 0.3170188387650512141, 0.3333333333333333703, 0.3170188387650512141, 0.3333333333333333703, 0.3170188387650512141, 0.3333333333333333703, 0.3170188387650512141, 0.3333333333333333703, 0.3170188387650512141, 0.3333333333333333703, 0.3170188387650512141, 0.3333333333333333703, 0.3170188387650512141, 0.3333333333333333703, 0.3170188387650512141, 0.3333333333333333703, 0.3170188387650512141, 0.3333333333333333703, 0.3170188387650512141, 0.3333333333333333703, 0.3170188387650512141, 0.3333333333333333703, 0.3170188387650512141, 0.3333333333333333703, 0.3170188387650512141, 0.3333333333333333703, 0.3170188387650512141, 0.3333333333333333703, 0.3170188387650512141, 0.3333333333333333703, 0.3170188387650512141, 0.3333333333333333703, 0.3170188387650512141, 0.3333333333333333703, 0.3170188387650512141, 0.3333333333333333703, 0.3170188387650512141, 0.3333333333333333703, 0.3170188387650512141, 0.3333333333333333703, 0.3170188387650512141, 0.3333333333333333703, 0.3170188387650512141, 0.3333333333333333703, 0.3170188387650512141, 0.3333333333333333703, 0.3170188387650512141, 0.3333333333333333703, 0.3170188387650512141, 0.3333333333333333703, 0.3170188387650512141, 0.3333333333333333703, 0.3170188387650512141, 0.3333333333333333703, 0.3170188387650512141, 0.3333333333333333703, 0.3170188387650512141, 0.3333333333333333703),
 ( 0.3333333333333333703, 0.3170188387650512141, 0.3333333333333333703, 0.3170188387650512141, 0.3333333333333333703, 0.3170188387650512141, 0.3333333333333333703, 0.3170188387650512141, 0.3333333333333333703, 0.3170188387650512141, 0.3333333333333333703, 0.3170188387650512141, 0.3333333333333333703, 0.3170188387650512141, 0.3333333333333333703, 0.3170188387650512141, 0.3333333333333333703, 0.3170188387650512141, 0.3333333333333333703, 0.3170188387650512141, 0.3333333333333333703, 0.3170188387650512141, 0.3333333333333333703, 0.3170188387650512141, 0.3333333333333333703, 0.3170188387650512141, 0.3333333333333333703, 0.3170188387650512141, 0.3333333333333333703, 0.3170188387650512141, 0.3333333333333333703, 0.3170188387650512141, 0.3333333333333333703, 0.3170188387650512141, 0.3333333333333333703, 0.3170188387650512141, 0.3333333333333333703, 0.3170188387650512141, 0.3333333333333333703, 0.3170188387650512141, 0.3333333333333333703, 0.3170188387650512141, 0.3333333333333333703, 0.3170188387650512141, 0.3333333333333333703, 0.3170188387650512141, 0.3333333333333333703, 0.3170188387650512141, 0.3333333333333333703, 0.3170188387650512141, 0.3333333333333333703, 0.3170188387650512141, 0.3333333333333333703, 0.3170188387650512141, 0.3333333333333333703, 0.3170188387650512141, 0.3333333333333333703, 0.3170188387650512141, 0.3333333333333333703, 0.3170188387650512141, 0.3333333333333333703, 0.3170188387650512141, 0.3333333333333333703, 0.3170188387650512141, 0.3333333333333333703, 0.3170188387650512141, 0.3333333333333333703, 0.3170188387650512141, 0.3333333333333333703, 0.3170188387650512141, 0.3333333333333333703, 0.3170188387650512141, 0.3333333333333333703, 0.3170188387650512141, 0.3333333333333333703, 0.3170188387650512141, 0.3333333333333333703, 0.3170188387650512141, 0.3333333333333333703, 0.3170188387650512141, 0.3333333333333333703, 0.3170188387650512141, 0.3333333333333333703, 0.3170188387650512141, 0.3333333333333333703, 0.3170188387650512141, 0.3333333333333333703, 0.3170188387650512141, 0.3333333333333333703, 0.3170188387650512141, 0.3333333333333333703, 0.3170188387650512141, 0.3333333333333333703, 0.3170188387650512141, 0.3333333333333333703, 0.3170188387650512141, 0.3333333333333333703, 0.3170188387650512141, 0.3333333333333333703, 0.3170188387650512141, 0.3333333333333333703, 0.3170188387650512141, 0.3333333333333333703, 0.3170188387650512141, 0.3333333333333333703, 0.3170188387650512141, 0.3333333333333333703, 0.3170188387650512141, 0.3333333333333333703, 0.3170188387650512141, 0.3333333333333333703, 0.3170188387650512141, 0.3333333333333333703, 0.3170188387650512141, 0.3333333333333333703, 0.3170188387650512141, 0.3333333333333333703, 0.3170188387650512141, 0.3333333333333333703, 0.3170188387650512141, 0.3333333333333333703, 0.3170188387650512141, 0.3333333333333333703, 0.3170188387650512141, 0.3333333333333333703, 0.3170188387650512141, 0.3333333333333333703, 0.3170188387650512141, 0.3333333333333333703, 0.3170188387650512141, 0.3333333333333333703, 0.3170188387650512141, 0.3333333333333333703, 0.3170188387650512141, 0.3333333333333333703, 0.3170188387650512141, 0.3333333333333333703, 0.3170188387650512141, 0.3333333333333333703, 0.3170188387650512141, 0.3333333333333333703, 0.3170188387650512141, 0.3333333333333333703, 0.3170188387650512141, 0.3333333333333333703, 0.3170188387650512141, 0.3333333333333333703, 0.3170188387650512141, 0.3333333333333333703, 0.3170188387650512141, 0.3333333333333333703, 0.3170188387650512141, 0.3333333333333333703, 0.3170188387650512141, 0.3333333333333333703, 0.3170188387650512141, 0.3333333333333333703, 0.3170188387650512141, 0.3333333333333333703, 0.3170188387650512141, 0.3333333333333333703, 0.3170188387650512141, 0.3333333333333333703, 0.3170188387650512141, 0.3333333333333333703, 0.3170188387650512141, 0.3333333333333333703, 0.3170188387650512141, 0.3333333333333333703, 0.3170188387650512141, 0.3333333333333333703, 0.3170188387650512141, 0.3333333333333333703, 0.3170188387650512141, 0.3333333333333333703, 0.3170188387650512141, 0.3333333333333333703, 0.3170188387650512141, 0.3333333333333333703, 0.3170188387650512141, 0.3333333333333333703, 0.3170188387650512141, 0.3333333333333333703, 0.3170188387650512141, 0.3333333333333333703, 0.3170188387650512141, 0.3333333333333333703, 0.3170188387650512141, 0.3333333333333333703, 0.3170188387650512141, 0.3333333333333333703, 0.3170188387650512141, 0.3333333333333333703, 0.3170188387650512141, 0.3333333333333333703, 0.3170188387650512141, 0.3333333333333333703, 0.3170188387650512141, 0.3333333333333333703, 0.3170188387650512141, 0.3333333333333333703, 0.3170188387650512141, 0.3333333333333333703, 0.3170188387650512141, 0.3333333333333333703, 0.3170188387650512141, 0.3333333333333333703, 0.3170188387650512141, 0.3333333333333333703, 0.3170188387650512141, 0.3333333333333333703, 0.3170188387650512141, 0.3333333333333333703, 0.3170188387650512141, 0.3333333333333333703, 0.3170188387650512141, 0.3333333333333333703, 0.3170188387650512141, 0.3333333333333333703, 0.3170188387650512141, 0.3333333333333333703, 0.3170188387650512141, 0.3333333333333333703, 0.3170188387650512141, 0.3333333333333333703, 0.3170188387650512141, 0.3333333333333333703, 0.3170188387650512141, 0.3333333333333333703, 0.3170188387650512141, 0.3333333333333333703, 0.3170188387650512141, 0.3333333333333333703, 0.3170188387650512141, 0.3333333333333333703, 0.3170188387650512141, 0.3333333333333333703, 0.3170188387650512141, 0.3333333333333333703, 0.3170188387650512141, 0.3333333333333333703, 0.3170188387650512141, 0.3333333333333333703, 0.3170188387650512141, 0.3333333333333333703, 0.3170188387650512141, 0.3333333333333333703, 0.3170188387650512141, 0.3333333333333333703, 0.3170188387650512141, 0.3333333333333333703, 0.3170188387650512141, 0.3333333333333333703, 0.3170188387650512141, 0.3333333333333333703, 0.3170188387650512141, 0.3333333333333333703, 0.3170188387650512141, 0.3333333333333333703, 0.3170188387650512141, 0.3333333333333333703, 0.3170188387650512141, 0.3333333333333333703, 0.3170188387650512141, 0.3333333333333333703, 0.3170188387650512141, 0.3333333333333333703, 0.3170188387650512141, 0.3333333333333333703, 0.3170188387650512141, 0.3333333333333333703, 0.3170188387650512141, 0.3333333333333333703, 0.3170188387650512141, 0.3333333333333333703, 0.3170188387650512141, 0.3333333333333333703, 0.3170188387650512141, 0.3333333333333333703, 0.3170188387650512141, 0.3333333333333333703, 0.3170188387650512141, 0.3333333333333333703, 0.3170188387650512141, 0.3333333333333333703, 0.3170188387650512141, 0.3333333333333333703, 0.3170188387650512141, 0.3333333333333333703, 0.3170188387650512141, 0.3333333333333333703, 0.3170188387650512141, 0.3333333333333333703, 0.3170188387650512141, 0.3333333333333333703, 0.3170188387650512141, 0.3333333333333333703, 0.3170188387650512141, 0.3333333333333333703, 0.3170188387650512141, 0.3333333333333333703, 0.3170188387650512141, 0.3333333333333333703, 0.3170188387650512141, 0.3333333333333333703, 0.3170188387650512141, 0.3333333333333333703, 0.3170188387650512141, 0.3333333333333333703, 0.3170188387650512141, 0.3333333333333333703),
 ( 1.000000000000000000, 0.9510565162951535312, 1.000000000000000000, 0.9510565162951535312, 1.000000000000000000, 0.9510565162951535312, 1.000000000000000000, 0.9510565162951535312, 1.000000000000000000, 0.9510565162951535312, 1.000000000000000000, 0.9510565162951535312, 1.000000000000000000, 0.9510565162951535312, 1.000000000000000000, 0.9510565162951535312, 1.000000000000000000, 0.9510565162951535312, 1.000000000000000000, 0.9510565162951535312, 1.000000000000000000, 0.9510565162951535312, 1.000000000000000000, 0.9510565162951535312, 1.000000000000000000, 0.9510565162951535312, 1.000000000000000000, 0.9510565162951535312, 1.000000000000000000, 0.9510565162951535312, 1.000000000000000000, 0.9510565162951535312, 1.000000000000000000, 0.9510565162951535312, 1.000000000000000000, 0.9510565162951535312, 1.000000000000000000, 0.9510565162951535312, 1.000000000000000000, 0.9510565162951535312, 1.000000000000000000, 0.9510565162951535312, 1.000000000000000000, 0.9510565162951535312, 1.000000000000000000, 0.9510565162951535312, 1.000000000000000000, 0.9510565162951535312, 1.000000000000000000, 0.9510565162951535312, 1.000000000000000000, 0.9510565162951535312, 1.000000000000000000, 0.9510565162951535312, 1.000000000000000000, 0.9510565162951535312, 1.000000000000000000, 0.9510565162951535312, 1.000000000000000000, 0.9510565162951535312, 1.000000000000000000, 0.9510565162951535312, 1.000000000000000000, 0.9510565162951535312, 1.000000000000000000, 0.9510565162951535312, 1.000000000000000000, 0.9510565162951535312, 1.000000000000000000, 0.9510565162951535312, 1.000000000000000000, 0.9510565162951535312, 1.000000000000000000, 0.9510565162951535312, 1.000000000000000000, 0.9510565162951535312, 1.000000000000000000, 0.9510565162951535312, 1.000000000000000000, 0.9510565162951535312, 1.000000000000000000, 0.9510565162951535312, 1.000000000000000000, 0.9510565162951535312, 1.000000000000000000, 0.9510565162951535312, 1.000000000000000000, 0.9510565162951535312, 1.000000000000000000, 0.9510565162951535312, 1.000000000000000000, 0.9510565162951535312, 1.000000000000000000, 0.9510565162951535312, 1.000000000000000000, 0.9510565162951535312, 1.000000000000000000, 0.9510565162951535312, 1.000000000000000000, 0.9510565162951535312, 1.000000000000000000, 0.9510565162951535312, 1.000000000000000000, 0.9510565162951535312, 1.000000000000000000, 0.9510565162951535312, 1.000000000000000000, 0.9510565162951535312, 1.000000000000000000, 0.9510565162951535312, 1.000000000000000000, 0.9510565162951535312, 1.000000000000000000, 0.9510565162951535312, 1.000000000000000000, 0.9510565162951535312, 1.000000000000000000, 0.9510565162951535312, 1.000000000000000000, 0.9510565162951535312, 1.000000000000000000, 0.9510565162951535312, 1.000000000000000000, 0.9510565162951535312, 1.000000000000000000, 0.9510565162951535312, 1.000000000000000000, 0.9510565162951535312, 1.000000000000000000, 0.9510565162951535312, 1.000000000000000000, 0.9510565162951535312, 1.000000000000000000, 0.9510565162951535312, 1.000000000000000000, 0.9510565162951535312, 1.000000000000000000, 0.9510565162951535312, 1.000000000000000000, 0.9510565162951535312, 1.000000000000000000, 0.9510565162951535312, 1.000000000000000000, 0.9510565162951535312, 1.000000000000000000, 0.9510565162951535312, 1.000000000000000000, 0.9510565162951535312, 1.000000000000000000, 0.9510565162951535312, 1.000000000000000000, 0.9510565162951535312, 1.000000000000000000, 0.9510565162951535312, 1.000000000000000000, 0.9510565162951535312, 1.000000000000000000, 0.9510565162951535312, 1.000000000000000000, 0.9510565162951535312, 1.000000000000000000, 0.9510565162951535312, 1.000000000000000000, 0.9510565162951535312, 1.000000000000000000, 0.9510565162951535312, 1.000000000000000000, 0.9510565162951535312, 1.000000000000000000, 0.9510565162951535312, 1.000000000000000000, 0.9510565162951535312, 1.000000000000000000, 0.9510565162951535312, 1.000000000000000000, 0.9510565162951535312, 1.000000000000000000, 0.9510565162951535312, 1.000000000000000000, 0.9510565162951535312, 1.000000000000000000, 0.9510565162951535312, 1.000000000000000000, 0.9510565162951535312, 1.000000000000000000, 0.9510565162951535312, 1.000000000000000000, 0.9510565162951535312, 1.000000000000000000, 0.9510565162951535312, 1.000000000000000000, 0.9510565162951535312, 1.000000000000000000, 0.9510565162951535312, 1.000000000000000000, 0.9510565162951535312, 1.000000000000000000, 0.9510565162951535312, 1.000000000000000000, 0.9510565162951535312, 1.000000000000000000, 0.9510565162951535312, 1.000000000000000000, 0.9510565162951535312, 1.000000000000000000, 0.9510565162951535312, 1.000000000000000000, 0.9510565162951535312, 1.000000000000000000, 0.9510565162951535312, 1.000000000000000000, 0.9510565162951535312, 1.000000000000000000, 0.9510565162951535312, 1.000000000000000000, 0.9510565162951535312, 1.000000000000000000, 0.9510565162951535312, 1.000000000000000000, 0.9510565162951535312, 1.000000000000000000, 0.9510565162951535312, 1.000000000000000000, 0.9510565162951535312, 1.000000000000000000, 0.9510565162951535312, 1.000000000000000000, 0.9510565162951535312, 1.000000000000000000, 0.9510565162951535312, 1.000000000000000000, 0.9510565162951535312, 1.000000000000000000, 0.9510565162951535312, 1.000000000000000000, 0.9510565162951535312, 1.000000000000000000, 0.9510565162951535312, 1.000000000000000000, 0.9510565162951535312, 1.000000000000000000, 0.9510565162951535312, 1.000000000000000000, 0.9510565162951535312, 1.000000000000000000, 0.9510565162951535312, 1.000000000000000000, 0.9510565162951535312, 1.000000000000000000, 0.9510565162951535312, 1.000000000000000000, 0.9510565162951535312, 1.000000000000000000, 0.9510565162951535312, 1.000000000000000000, 0.9510565162951535312, 1.000000000000000000, 0.9510565162951535312, 1.000000000000000000, 0.9510565162951535312, 1.000000000000000000, 0.9510565162951535312, 1.000000000000000000, 0.9510565162951535312, 1.000000000000000000, 0.9510565162951535312, 1.000000000000000000, 0.9510565162951535312, 1.000000000000000000, 0.9510565162951535312, 1.000000000000000000, 0.9510565162951535312, 1.000000000000000000, 0.9510565162951535312, 1.000000000000000000, 0.9510565162951535312, 1.000000000000000000, 0.9510565162951535312, 1.000000000000000000, 0.9510565162951535312, 1.000000000000000000, 0.9510565162951535312, 1.000000000000000000, 0.9510565162951535312, 1.000000000000000000, 0.9510565162951535312, 1.000000000000000000, 0.9510565162951535312, 1.000000000000000000, 0.9510565162951535312, 1.000000000000000000, 0.9510565162951535312, 1.000000000000000000, 0.9510565162951535312, 1.000000000000000000, 0.9510565162951535312, 1.000000000000000000, 0.9510565162951535312, 1.000000000000000000, 0.9510565162951535312, 1.000000000000000000, 0.9510565162951535312, 1.000000000000000000, 0.9510565162951535312, 1.000000000000000000, 0.9510565162951535312, 1.000000000000000000, 0.9510565162951535312, 1.000000000000000000, 0.9510565162951535312, 1.000000000000000000) ) ) 
 REPRESENTATION_ITEM ( '' )  SURFACE ( )  );
#10462 = CARTESIAN_POINT ( 'NONE',  ( 37.31647492878124694, -24.30384086642191122, 72.03616607671141026 ) ) ;
#10463 = CARTESIAN_POINT ( 'NONE',  ( 38.82593461698262871, -10.91368208888609992, 69.62690120949091011 ) ) ;
#10464 = VERTEX_POINT ( 'NONE', #22988 ) ;
#10465 = CARTESIAN_POINT ( 'NONE',  ( 30.81606138205706102, -34.13844651005150155, 70.48338531520533934 ) ) ;
#10466 = ADVANCED_FACE ( 'NONE', ( #5601 ), #7795, .T. ) ;
#10467 = ORIENTED_EDGE ( 'NONE', *, *, #17300, .F. ) ;
#10468 = ADVANCED_BREP_SHAPE_REPRESENTATION ( '', ( #25444, #2000 ), #6728 ) ;
#10469 = CARTESIAN_POINT ( 'NONE',  ( 39.95015449827720744, -13.00384086642191228, 71.96809898377887293 ) ) ;
#10470 = CARTESIAN_POINT ( 'NONE',  ( 45.81606138205700063, 40.39281886181299797, 84.30501292736984453 ) ) ;
#10471 = AXIS2_PLACEMENT_3D ( 'NONE', #18468, #16522, #12936 ) ;
#10472 = CARTESIAN_POINT ( 'NONE',  ( 40.14115730948191185, -8.513682088886104893, 71.32335560751961623 ) ) ;
#10473 = ORIENTED_EDGE ( 'NONE', *, *, #15691, .T. ) ;
#10474 = CARTESIAN_POINT ( 'NONE',  ( 39.73277004305198545, -16.21368208888610596, 73.23812341099225875 ) ) ;
#10475 = ORIENTED_EDGE ( 'NONE', *, *, #11356, .F. ) ;
#10476 = CARTESIAN_POINT ( 'NONE',  ( 36.31606138205700063, -7.108955154158179468, 82.62193108360246185 ) ) ;
#10477 = DIRECTION ( 'NONE',  ( 0.000000000000000000, 0.6568589528324747517, -0.7540134720837717852 ) ) ;
#10478 = CARTESIAN_POINT ( 'NONE',  ( 39.51027997493896748, -21.10384086642191193, 71.43714994484032843 ) ) ;
#10479 = ORIENTED_EDGE ( 'NONE', *, *, #584, .T. ) ;
#10480 = ORIENTED_EDGE ( 'NONE', *, *, #6293, .F. ) ;
#10481 = LINE ( 'NONE', #4674, #19538 ) ;
#10482 = VECTOR ( 'NONE', #21688, 1000.000000000000000 ) ;
#10483 = LINE ( 'NONE', #14462, #12072 ) ;
#10484 = CARTESIAN_POINT ( 'NONE',  ( 39.12911128074872380, -21.50384086642191406, 69.06206559358665231 ) ) ;
#10485 = CARTESIAN_POINT ( 'NONE',  ( 43.81606138205700063, -34.55876147765400930, 73.30501292737011454 ) ) ;
#10486 = CARTESIAN_POINT ( 'NONE',  ( 37.80618814713140097, -25.91368208888610880, 73.13360434286902034 ) ) ;
#10487 = FACE_OUTER_BOUND ( 'NONE', #10973, .T. ) ;
#10488 = CARTESIAN_POINT ( 'NONE',  ( 36.31606138205699352, -10.61256217995208928, 37.48782943861662886 ) ) ;
#10489 = ORIENTED_EDGE ( 'NONE', *, *, #18787, .F. ) ;
#10490 = CARTESIAN_POINT ( 'NONE',  ( 45.81606138205705037, -30.46100403034029114, 72.05704881431049103 ) ) ;
#10491 = VECTOR ( 'NONE', #2242, 1000.000000000000227 ) ;
#10492 = DIRECTION ( 'NONE',  ( 0.000000000000000000, 1.000000000000000000, 0.000000000000000000 ) ) ;
#10493 = CARTESIAN_POINT ( 'NONE',  ( 36.68196826583682935, -16.00384086642191050, 70.79240656858107172 ) ) ;
#10494 = DIRECTION ( 'NONE',  ( 1.000000000000000000, 0.000000000000000000, 0.000000000000000000 ) ) ;
#10495 = DIRECTION ( 'NONE',  ( 0.000000000000000000, -0.8967398287344626739, -0.4425581086832399147 ) ) ;
#10496 = LINE ( 'NONE', #2734, #19701 ) ;
#10497 = EDGE_CURVE ( 'NONE', #8968, #19348, #15388, .T. ) ;
#10498 = CARTESIAN_POINT ( 'NONE',  ( 35.81606138205700063, -31.05876147765399864, 75.30501292737010033 ) ) ;
#10499 = CARTESIAN_POINT ( 'NONE',  ( 37.69225076346193504, -1.803840866421911215, 70.42958956619168021 ) ) ;
#10500 = CARTESIAN_POINT ( 'NONE',  ( 33.33121445922205339, -32.87633672316712108, 59.29685926994373091 ) ) ;
#10501 = VERTEX_POINT ( 'NONE', #13220 ) ;
#10502 = CARTESIAN_POINT ( 'NONE',  ( 36.68196826583682935, -25.61368208888610454, 71.96809898377887293 ) ) ;
#10503 = ORIENTED_EDGE ( 'NONE', *, *, #6269, .F. ) ;
#10504 = ORIENTED_EDGE ( 'NONE', *, *, #24901, .F. ) ;
#10505 = DIRECTION ( 'NONE',  ( 0.000000000000000000, 3.469446951953611033E-15, 1.000000000000000000 ) ) ;
#10506 = DIRECTION ( 'NONE',  ( -1.000000000000000000, 3.083952846180990083E-15, -9.251858538542970050E-30 ) ) ;
#10507 = CARTESIAN_POINT ( 'NONE',  ( 37.21915885897815457, -3.413682088886101251, 71.08074471024443142 ) ) ;
#10508 = CARTESIAN_POINT ( 'NONE',  ( 39.51027997493896748, -2.513682088886099564, 71.32335560751961623 ) ) ;
#10509 = ORIENTED_EDGE ( 'NONE', *, *, #1221, .T. ) ;
#10510 = ORIENTED_EDGE ( 'NONE', *, *, #7509, .T. ) ;
#10511 = CARTESIAN_POINT ( 'NONE',  ( 31.56606138205707168, -38.42645682328038248, 63.90656833300437256 ) ) ;
#10512 = LINE ( 'NONE', #22353, #23132 ) ;
#10513 = DIRECTION ( 'NONE',  ( -7.071067811865460542E-16, 0.4341746501209495790, 0.9008287146801832179 ) ) ;
#10514 = CARTESIAN_POINT ( 'NONE',  ( 37.80618814713138676, -13.70384086642190979, 69.62690120949091011 ) ) ;
#10515 = CIRCLE ( 'NONE', #17097, 0.7499999999999983347 ) ;
#10516 = EDGE_CURVE ( 'NONE', #2496, #19007, #5503, .T. ) ;
#10517 = DIRECTION ( 'NONE',  ( 1.000000000000000000, 0.000000000000000000, 0.000000000000000000 ) ) ;
#10518 = ADVANCED_FACE ( 'NONE', ( #21314 ), #23239, .T. ) ;
#10519 = CARTESIAN_POINT ( 'NONE',  ( 42.81606138205700063, 22.19123852234703520, 80.30501292736994401 ) ) ;
#10520 = EDGE_CURVE ( 'NONE', #1727, #15791, #24902, .T. ) ;
#10521 = ORIENTED_EDGE ( 'NONE', *, *, #23865, .T. ) ;
#10522 = ORIENTED_EDGE ( 'NONE', *, *, #13344, .F. ) ;
#10523 = EDGE_CURVE ( 'NONE', #19561, #5208, #9493, .T. ) ;
#10524 = EDGE_CURVE ( 'NONE', #11291, #120, #3414, .T. ) ;
#10525 = ORIENTED_EDGE ( 'NONE', *, *, #7228, .F. ) ;
#10526 = LINE ( 'NONE', #24653, #4251 ) ;
#10527 = CARTESIAN_POINT ( 'NONE',  ( 39.75915168707250302, -10.71368208888610063, 70.26145752964255564 ) ) ;
#10528 = CARTESIAN_POINT ( 'NONE',  ( 39.95532413685785400, -29.10876147765399580, 71.32982406108487794 ) ) ;
#10529 = DIRECTION ( 'NONE',  ( -1.301042606982603842E-16, 0.000000000000000000, -1.000000000000000000 ) ) ;
#10530 = ORIENTED_EDGE ( 'NONE', *, *, #13047, .T. ) ;
#10531 = CARTESIAN_POINT ( 'NONE',  ( 36.31606138205702194, -20.48383445069737618, 23.59578481461660004 ) ) ;
#10532 = EDGE_CURVE ( 'NONE', #8151, #12953, #24819, .T. ) ;
#10533 = EDGE_CURVE ( 'NONE', #1877, #13391, #17012, .T. ) ;
#10534 = DIRECTION ( 'NONE',  ( 0.000000000000000000, -0.6568589528324746407, 0.7540134720837717852 ) ) ;
#10535 = LINE ( 'NONE', #18012, #14714 ) ;
#10536 = FACE_OUTER_BOUND ( 'NONE', #20667, .T. ) ;
#10537 = ORIENTED_EDGE ( 'NONE', *, *, #12413, .T. ) ;
#10538 = ORIENTED_EDGE ( 'NONE', *, *, #8860, .F. ) ;
#10539 = CARTESIAN_POINT ( 'NONE',  ( 45.81606138205700063, 0.1601050959395486362, 68.80395113470939350 ) ) ;
#10540 = CARTESIAN_POINT ( 'NONE',  ( 36.36258059203030513, 0.09615913357808798800, 69.89063713639259845 ) ) ;
#10541 = CARTESIAN_POINT ( 'NONE',  ( 37.38336156205274818, -25.71368208888610241, 72.12822762946747446 ) ) ;
#10542 = ORIENTED_EDGE ( 'NONE', *, *, #6590, .F. ) ;
#10543 = EDGE_CURVE ( 'NONE', #11605, #1915, #14144, .T. ) ;
#10544 = ORIENTED_EDGE ( 'NONE', *, *, #594, .F. ) ;
#10545 = DIRECTION ( 'NONE',  ( 1.000000000000000000, 2.751104698760144965E-15, -1.228345504986737969E-16 ) ) ;
#10546 = CARTESIAN_POINT ( 'NONE',  ( 38.37017380507020192, -4.013682088886107557, 73.11602215082118050 ) ) ;
#10547 = CARTESIAN_POINT ( 'NONE',  ( 38.26194895904384197, 1.396159133578087186, 72.51602215082118619 ) ) ;
#10548 = DIRECTION ( 'NONE',  ( 0.000000000000000000, 0.000000000000000000, -1.000000000000000000 ) ) ;
#10549 = CARTESIAN_POINT ( 'NONE',  ( 37.61123632939165873, -5.913682088886105248, 73.73360434286902887 ) ) ;
#10550 = CARTESIAN_POINT ( 'NONE',  ( 31.56606138205708589, -41.96692169274629691, 71.08048696288007307 ) ) ;
#10551 = VECTOR ( 'NONE', #9297, 1000.000000000000114 ) ;
#10552 = LINE ( 'NONE', #18287, #8756 ) ;
#10553 = CARTESIAN_POINT ( 'NONE',  ( 32.56606138205700773, 43.35512946304240245, 82.37823623207322044 ) ) ;
#10554 = LINE ( 'NONE', #8618, #17385 ) ;
#10555 = CARTESIAN_POINT ( 'NONE',  ( 40.31606138205700773, -6.984061928592629975, 82.64107068069698414 ) ) ;
#10556 = EDGE_CURVE ( 'NONE', #10887, #20815, #17461, .T. ) ;
#10557 = DIRECTION ( 'NONE',  ( 0.000000000000000000, 2.999999999999999839E-15, 1.000000000000000000 ) ) ;
#10558 = VERTEX_POINT ( 'NONE', #11410 ) ;
#10559 = CARTESIAN_POINT ( 'NONE',  ( 38.31606138205700063, -22.22127907754186893, 75.29996292736998953 ) ) ;
#10560 = CARTESIAN_POINT ( 'NONE',  ( 46.81606138205706458, -34.54722833698617990, 70.28164373264664277 ) ) ;
#10561 = ORIENTED_EDGE ( 'NONE', *, *, #15581, .F. ) ;
#10562 = ORIENTED_EDGE ( 'NONE', *, *, #231, .F. ) ;
#10563 = CARTESIAN_POINT ( 'NONE',  ( 39.73277004305197124, -17.40384086642191264, 69.52238214136768590 ) ) ;
#10564 = EDGE_CURVE ( 'NONE', #4853, #14092, #17328, .T. ) ;
#10565 = CARTESIAN_POINT ( 'NONE',  ( 37.25202387243752611, -25.21368208888610241, 70.00779233799262613 ) ) ;
#10566 = EDGE_CURVE ( 'NONE', #6502, #24213, #7667, .T. ) ;
#10567 = CARTESIAN_POINT ( 'NONE',  ( 38.31606138205700063, 29.20347903359266084, 94.80501292737000085 ) ) ;
#10568 = DIRECTION ( 'NONE',  ( 0.000000000000000000, -0.7516416929448823669, -0.6595716529892345914 ) ) ;
#10569 = ORIENTED_EDGE ( 'NONE', *, *, #4361, .F. ) ;
#10570 = PLANE ( 'NONE',  #17503 ) ;
#10571 = CARTESIAN_POINT ( 'NONE',  ( 40.31606138205700773, -12.40281258615395821, 20.95421293576468358 ) ) ;
#10572 = CARTESIAN_POINT ( 'NONE',  ( 39.12911128074873801, -26.11368208888610809, 73.69843995877326392 ) ) ;
#10573 = AXIS2_PLACEMENT_3D ( 'NONE', #23899, #8202, #6142 ) ;
#10574 = DIRECTION ( 'NONE',  ( 1.000000000000000000, 1.156482317317870344E-15, 0.000000000000000000 ) ) ;
#10575 = FACE_OUTER_BOUND ( 'NONE', #3636, .T. ) ;
#10576 = CIRCLE ( 'NONE', #24936, 1.500000000000006217 ) ;
#10577 = VECTOR ( 'NONE', #13945, 1000.000000000000000 ) ;
#10578 = CARTESIAN_POINT ( 'NONE',  ( 39.98359781491296161, -6.413682088886103472, 71.86517103874048473 ) ) ;
#10579 = FACE_OUTER_BOUND ( 'NONE', #8932, .T. ) ;
#10580 = CARTESIAN_POINT ( 'NONE',  ( 36.68196826583682935, -21.61368208888610454, 71.96809898377888715 ) ) ;
#10581 = DIRECTION ( 'NONE',  ( 0.000000000000000000, -0.6595716529892419189, 0.7516416929448759277 ) ) ;
#10582 = DIRECTION ( 'NONE',  ( 1.000000000000000000, 2.999999999999999839E-15, 0.000000000000000000 ) ) ;
#10583 = CARTESIAN_POINT ( 'NONE',  ( 38.37017380507018771, -27.60384086642191548, 70.24448340153875847 ) ) ;
#10584 = CARTESIAN_POINT ( 'NONE',  ( 40.14115730948191185, -12.51368208888610489, 71.32335560751960202 ) ) ;
#10585 = ORIENTED_EDGE ( 'NONE', *, *, #23168, .F. ) ;
#10586 = DIRECTION ( 'NONE',  ( 0.000000000000000000, 0.000000000000000000, 1.000000000000000000 ) ) ;
#10587 = VERTEX_POINT ( 'NONE', #15262 ) ;
#10588 = AXIS2_PLACEMENT_3D ( 'NONE', #3878, #11244, #1433 ) ;
#10589 = EDGE_CURVE ( 'NONE', #22719, #8502, #23111, .T. ) ;
#10590 = CARTESIAN_POINT ( 'NONE',  ( 40.14115730948191185, -9.103840866421911926, 71.43714994484034264 ) ) ;
#10591 = CARTESIAN_POINT ( 'NONE',  ( 44.81606138205700063, -36.55876147765401640, 71.30501292737011454 ) ) ;
#10592 = EDGE_CURVE ( 'NONE', #4563, #18120, #13593, .T. ) ;
#10593 = AXIS2_PLACEMENT_3D ( 'NONE', #16520, #1057, #16658 ) ;
#10594 = VECTOR ( 'NONE', #7300, 1000.000000000000000 ) ;
#10595 = EDGE_CURVE ( 'NONE', #1793, #6631, #17432, .T. ) ;
#10596 = CARTESIAN_POINT ( 'NONE',  ( 40.14115730948191185, -6.513682088886103116, 71.32335560751961623 ) ) ;
#10597 = VERTEX_POINT ( 'NONE', #21696 ) ;
#10598 = CARTESIAN_POINT ( 'NONE',  ( 40.26954217208371034, -12.71368208888610241, 69.89063713639258424 ) ) ;
#10599 = EDGE_LOOP ( 'NONE', ( #13786, #18127, #9217, #23110 ) ) ;
#10600 = CYLINDRICAL_SURFACE ( 'NONE', #17269, 12.59999999999999964 ) ;
#10601 = CARTESIAN_POINT ( 'NONE',  ( 40.56606138205696510, -1.522470315718718270, 0.9921758631592225708 ) ) ;
#10602 = CARTESIAN_POINT ( 'NONE',  ( 37.31647492878124694, -10.30384086642191122, 72.03616607671141026 ) ) ;
#10603 = FACE_OUTER_BOUND ( 'NONE', #9393, .T. ) ;
#10604 = EDGE_LOOP ( 'NONE', ( #9670, #21631, #908, #822 ) ) ;
#10605 = CARTESIAN_POINT ( 'NONE',  ( 44.81606138205700063, 41.44123852234599781, 75.30501292736987295 ) ) ;
#10606 = CARTESIAN_POINT ( 'NONE',  ( 32.81606138205700773, 44.92314894770293421, 79.37823623207320622 ) ) ;
#10607 = CARTESIAN_POINT ( 'NONE',  ( 36.11133435605973574, -18.00384086642191050, 70.60699637195608602 ) ) ;
#10608 = DIRECTION ( 'NONE',  ( 0.000000000000000000, -1.000000000000000000, 2.999999999999999839E-15 ) ) ;
#10609 = CARTESIAN_POINT ( 'NONE',  ( 38.37017380507020192, -24.01368208888610667, 73.11602215082115208 ) ) ;
#10610 = CARTESIAN_POINT ( 'NONE',  ( 43.79080625344859357, -32.95845724189726411, 59.23979596822106686 ) ) ;
#10611 = EDGE_CURVE ( 'NONE', #11314, #6791, #7972, .T. ) ;
#10612 = CARTESIAN_POINT ( 'NONE',  ( 44.81606138205700063, -34.55876147765400930, 73.30501292737011454 ) ) ;
#10613 = VECTOR ( 'NONE', #22824, 1000.000000000000000 ) ;
#10614 = EDGE_LOOP ( 'NONE', ( #8352, #17595, #15254, #20413, #8833, #8992 ) ) ;
#10615 = VECTOR ( 'NONE', #11150, 1000.000000000000000 ) ;
#10616 = VECTOR ( 'NONE', #23906, 1000.000000000000000 ) ;
#10617 = DIRECTION ( 'NONE',  ( 0.000000000000000000, 0.5706330172266920187, -0.8212051873014210024 ) ) ;
#10618 = CARTESIAN_POINT ( 'NONE',  ( 32.81606138205700773, 4.124002793203064066, 6.312068993173404863 ) ) ;
#10619 = CARTESIAN_POINT ( 'NONE',  ( 39.95015449827720744, -15.00384086642191228, 71.96809898377887293 ) ) ;
#10620 = DIRECTION ( 'NONE',  ( 1.000000000000000000, 0.000000000000000000, 0.000000000000000000 ) ) ;
#10621 = CARTESIAN_POINT ( 'NONE',  ( 40.81606138205700773, -31.05876147765399864, 74.30501292737010033 ) ) ;
#10622 = FACE_OUTER_BOUND ( 'NONE', #25362, .T. ) ;
#10623 = CARTESIAN_POINT ( 'NONE',  ( 38.41621794735363693, -35.10729675983900222, 83.30501292737010033 ) ) ;
#10624 = CARTESIAN_POINT ( 'NONE',  ( 37.25260217561390874, -2.003840866421909617, 70.97781676520604321 ) ) ;
#10625 = CARTESIAN_POINT ( 'NONE',  ( 31.81606138205700418, 34.87886987267149408, 81.44836866983821722 ) ) ;
#10626 = ORIENTED_EDGE ( 'NONE', *, *, #10533, .F. ) ;
#10627 = CARTESIAN_POINT ( 'NONE',  ( 37.80618814713140097, -27.91368208888610880, 73.13360434286902034 ) ) ;
#10628 = VERTEX_POINT ( 'NONE', #21949 ) ;
#10629 = ORIENTED_EDGE ( 'NONE', *, *, #666, .T. ) ;
#10630 = CIRCLE ( 'NONE', #22531, 1.750000000000001554 ) ;
#10631 = CARTESIAN_POINT ( 'NONE',  ( 42.56606138205700063, 2.740850673309605412, 6.112030963703427133 ) ) ;
#10632 = DIRECTION ( 'NONE',  ( 1.000000000000000000, 2.751104698760144965E-15, -1.228345504986739201E-16 ) ) ;
#10633 = CARTESIAN_POINT ( 'NONE',  ( 39.37952058850012804, -29.00384086642191406, 71.78268878715390144 ) ) ;
#10634 = AXIS2_PLACEMENT_3D ( 'NONE', #6857, #5061, #13052 ) ;
#10635 = AXIS2_PLACEMENT_3D ( 'NONE', #25326, #21481, #3829 ) ;
#10636 = CARTESIAN_POINT ( 'NONE',  ( 37.12184278917507640, 0.4863179111138996036, 71.43714994484035685 ) ) ;
#10637 = ORIENTED_EDGE ( 'NONE', *, *, #6581, .T. ) ;
#10638 = ORIENTED_EDGE ( 'NONE', *, *, #5767, .T. ) ;
#10639 = CARTESIAN_POINT ( 'NONE',  ( 31.81606138205700418, -38.55876147765401640, 71.30501292737012875 ) ) ;
#10640 = LINE ( 'NONE', #2505, #87 ) ;
#10641 = VERTEX_POINT ( 'NONE', #10354 ) ;
#10642 = DIRECTION ( 'NONE',  ( 0.000000000000000000, -0.3299742535181005021, 0.9439899321577387425 ) ) ;
#10643 = CARTESIAN_POINT ( 'NONE',  ( 38.82593461698265003, -10.70384086642191690, 73.13360434286904876 ) ) ;
#10644 = FILL_AREA_STYLE_COLOUR ( '', #17450 ) ;
#10645 = EDGE_CURVE ( 'NONE', #16518, #14083, #9983, .T. ) ;
#10646 = DIRECTION ( 'NONE',  ( 2.048868001712898319E-15, -0.6595716529892350355, 0.7516416929448821449 ) ) ;
#10647 = VERTEX_POINT ( 'NONE', #8050 ) ;
#10648 = ORIENTED_EDGE ( 'NONE', *, *, #4712, .F. ) ;
#10649 = CIRCLE ( 'NONE', #25003, 2.500000000000002220 ) ;
#10650 = ORIENTED_EDGE ( 'NONE', *, *, #17841, .F. ) ;
#10651 = CARTESIAN_POINT ( 'NONE',  ( 42.06606138205700063, 45.04446929126260102, 81.37823623207320622 ) ) ;
#10652 = CARTESIAN_POINT ( 'NONE',  ( 38.93415946300898867, -8.113682088886108090, 73.09843995877331224 ) ) ;
#10653 = ORIENTED_EDGE ( 'NONE', *, *, #8402, .F. ) ;
#10654 = CARTESIAN_POINT ( 'NONE',  ( 39.99513520555235857, -29.10876147765277722, 71.38080556064524274 ) ) ;
#10655 = LINE ( 'NONE', #18503, #23548 ) ;
#10656 = VECTOR ( 'NONE', #2616, 1000.000000000000000 ) ;
#10657 = FACE_OUTER_BOUND ( 'NONE', #19627, .T. ) ;
#10658 = CARTESIAN_POINT ( 'NONE',  ( 33.40064408022072939, 41.67000142393845152, 79.87823623207322044 ) ) ;
#10659 = CARTESIAN_POINT ( 'NONE',  ( 31.81606138205700418, 1.441238522345976714, 67.80501292737001506 ) ) ;
#10660 = EDGE_CURVE ( 'NONE', #18307, #17722, #8299, .T. ) ;
#10661 = EDGE_CURVE ( 'NONE', #23038, #21084, #4435, .T. ) ;
#10662 = CARTESIAN_POINT ( 'NONE',  ( 33.31606138205700773, -36.11063010576116739, 71.66210679335823386 ) ) ;
#10663 = EDGE_LOOP ( 'NONE', ( #8987, #9684, #22145, #2895 ) ) ;
#10664 = ORIENTED_EDGE ( 'NONE', *, *, #18399, .F. ) ;
#10665 = DIRECTION ( 'NONE',  ( -1.000000000000000000, 6.018531076210110289E-31, 1.734723475976804876E-16 ) ) ;
#10666 = CARTESIAN_POINT ( 'NONE',  ( 35.86008812008917346, -0.1038408664219142574, 71.32335560751961623 ) ) ;
#10667 = VECTOR ( 'NONE', #8372, 1000.000000000000227 ) ;
#10668 = EDGE_CURVE ( 'NONE', #21783, #2156, #3853, .T. ) ;
#10669 = CARTESIAN_POINT ( 'NONE',  ( 39.02742774030102879, -16.21368208888609885, 72.26730301774234988 ) ) ;
#10670 = ORIENTED_EDGE ( 'NONE', *, *, #1368, .F. ) ;
#10671 = ORIENTED_EDGE ( 'NONE', *, *, #13965, .F. ) ;
#10672 = LINE ( 'NONE', #2909, #17803 ) ;
#10673 = CARTESIAN_POINT ( 'NONE',  ( 37.25202387243752611, -1.213682088886100630, 70.00779233799264034 ) ) ;
#10674 = CARTESIAN_POINT ( 'NONE',  ( 37.33957961208645315, -27.80384086642191122, 69.94417936956671156 ) ) ;
#10675 = VECTOR ( 'NONE', #20152, 1000.000000000000000 ) ;
#10676 = CARTESIAN_POINT ( 'NONE',  ( 41.14099152588522657, -10.60718113818700026, 83.30501292737001506 ) ) ;
#10677 = ADVANCED_FACE ( 'NONE', ( #3925 ), #1972, .F. ) ;
#10678 = CARTESIAN_POINT ( 'NONE',  ( 39.12911128074873801, -8.113682088886108090, 73.69843995877330656 ) ) ;
#10679 = AXIS2_PLACEMENT_3D ( 'NONE', #3715, #15570, #25084 ) ;
#10680 = CARTESIAN_POINT ( 'NONE',  ( 45.81606138205707168, -37.26069504592553727, 64.48189387429259511 ) ) ;
#10681 = CARTESIAN_POINT ( 'NONE',  ( 33.31606138205700773, -29.06829118875199924, 75.80501292737000085 ) ) ;
#10682 = DIRECTION ( 'NONE',  ( 0.000000000000000000, -1.861251128379125107E-14, -1.000000000000000000 ) ) ;
#10683 = DIRECTION ( 'NONE',  ( -0.000000000000000000, -1.000000000000000000, 2.848211695852029218E-15 ) ) ;
#10684 = VECTOR ( 'NONE', #8180, 1000.000000000000114 ) ;
#10685 = PLANE ( 'NONE',  #11914 ) ;
#10686 = DIRECTION ( 'NONE',  ( 1.157642374584902751E-15, -0.3934158747763039088, 0.9193606199277819524 ) ) ;
#10687 = DIRECTION ( 'NONE',  ( 0.000000000000000000, 1.000000000000000000, -2.999999999999999839E-15 ) ) ;
#10688 = VECTOR ( 'NONE', #22174, 1000.000000000000000 ) ;
#10689 = EDGE_LOOP ( 'NONE', ( #21572, #11284, #11784, #4328 ) ) ;
#10690 = ADVANCED_FACE ( 'NONE', ( #15890 ), #23748, .T. ) ;
#10691 = DIRECTION ( 'NONE',  ( 0.000000000000000000, 0.6568589528324746407, -0.7540134720837716742 ) ) ;
#10692 = LINE ( 'NONE', #5008, #15246 ) ;
#10693 = ORIENTED_EDGE ( 'NONE', *, *, #15972, .F. ) ;
#10694 = ORIENTED_EDGE ( 'NONE', *, *, #11787, .F. ) ;
#10695 = CARTESIAN_POINT ( 'NONE',  ( 36.36258059203030513, -15.90384086642191264, 69.89063713639259845 ) ) ;
#10696 = ADVANCED_FACE ( 'NONE', ( #10231 ), #21019, .T. ) ;
#10697 = AXIS2_PLACEMENT_3D ( 'NONE', #5337, #21053, #17186 ) ;
#10698 = EDGE_CURVE ( 'NONE', #13966, #6270, #21821, .T. ) ;
#10699 = VECTOR ( 'NONE', #3518, 1000.000000000000000 ) ;
#10700 = CARTESIAN_POINT ( 'NONE',  ( 36.49096545463212493, -21.51368208888609956, 71.43714994484034264 ) ) ;
#10701 = FACE_OUTER_BOUND ( 'NONE', #2298, .T. ) ;
#10702 = VECTOR ( 'NONE', #20060, 1000.000000000000000 ) ;
#10703 = CARTESIAN_POINT ( 'NONE',  ( 40.31606138205702194, -20.30191568716148254, 23.22716926412510219 ) ) ;
#10704 = ORIENTED_EDGE ( 'NONE', *, *, #17686, .F. ) ;
#10705 = LINE ( 'NONE', #14806, #20375 ) ;
#10706 = CARTESIAN_POINT ( 'NONE',  ( 43.81606138205700063, 45.92314894770293421, 80.37823623207322044 ) ) ;
#10707 = EDGE_CURVE ( 'NONE', #14027, #22094, #21551, .T. ) ;
#10708 = CARTESIAN_POINT ( 'NONE',  ( 36.98690846071097127, 0.1961591335780874246, 69.45876917294177133 ) ) ;
#10709 = VERTEX_POINT ( 'NONE', #18217 ) ;
#10710 = FACE_OUTER_BOUND ( 'NONE', #1605, .T. ) ;
#10711 = CARTESIAN_POINT ( 'NONE',  ( 39.98359781491296161, -4.413682088886105248, 71.86517103874048473 ) ) ;
#10712 = DIRECTION ( 'NONE',  ( 0.000000000000000000, 0.6595716529892415858, -0.7516416929448761497 ) ) ;
#10713 = CARTESIAN_POINT ( 'NONE',  ( 37.33957961208646736, -17.81368208888611093, 72.81632618279321889 ) ) ;
#10714 = AXIS2_PLACEMENT_3D ( 'NONE', #9434, #17667, #21397 ) ;
#10715 = CARTESIAN_POINT ( 'NONE',  ( 38.44690133353662276, -22.22127907754186893, 75.80501292736997243 ) ) ;
#10716 = EDGE_CURVE ( 'NONE', #20891, #19678, #13098, .T. ) ;
#10717 = CARTESIAN_POINT ( 'NONE',  ( 33.81606138205700063, 2.191238522347003226, 70.30501292737000085 ) ) ;
#10718 = CARTESIAN_POINT ( 'NONE',  ( 39.31564783533279694, -19.30384086642191477, 70.72433947564853440 ) ) ;
#10719 = CARTESIAN_POINT ( 'NONE',  ( 38.93415946300897446, -4.113682088886107202, 73.09843995877331224 ) ) ;
#10720 = DIRECTION ( 'NONE',  ( 1.000000000000000000, 2.805550545906362824E-15, -9.596449257708899394E-17 ) ) ;
#10721 = ORIENTED_EDGE ( 'NONE', *, *, #6083, .F. ) ;
#10722 = CARTESIAN_POINT ( 'NONE',  ( 40.14115730948191185, -3.103840866421910150, 71.43714994484034264 ) ) ;
#10723 = DIRECTION ( 'NONE',  ( 0.000000000000000000, 0.5706330172266907974, -0.8212051873014217795 ) ) ;
#10724 = CARTESIAN_POINT ( 'NONE',  ( 38.82593461698262871, -4.913682088886100807, 69.62690120949091011 ) ) ;
#10725 = ORIENTED_EDGE ( 'NONE', *, *, #6628, .T. ) ;
#10726 = CARTESIAN_POINT ( 'NONE',  ( 36.89935272106204422, -11.21368208888610241, 69.52238214136768590 ) ) ;
#10727 = ORIENTED_EDGE ( 'NONE', *, *, #13193, .F. ) ;
#10728 = DIRECTION ( 'NONE',  ( -1.000000000000000000, 0.000000000000000000, 0.000000000000000000 ) ) ;
#10729 = CARTESIAN_POINT ( 'NONE',  ( 37.89291511884479036, -12.50384086642191228, 72.49843995877330372 ) ) ;
#10730 = DIRECTION ( 'NONE',  ( 1.000000000000000000, 0.000000000000000000, -0.000000000000000000 ) ) ;
#10731 = VECTOR ( 'NONE', #23511, 1000.000000000000000 ) ;
#10732 = ORIENTED_EDGE ( 'NONE', *, *, #15800, .T. ) ;
#10733 = CARTESIAN_POINT ( 'NONE',  ( 33.31606138205700773, -35.41471100349711065, 71.53682070832086026 ) ) ;
#10734 = DIRECTION ( 'NONE',  ( -1.000000000000000000, 0.000000000000000000, 0.000000000000000000 ) ) ;
#10735 = CARTESIAN_POINT ( 'NONE',  ( 36.07789103942399578, -14.20384086642191512, 72.05058123536544201 ) ) ;
#10736 = AXIS2_PLACEMENT_3D ( 'NONE', #9278, #3325, #18664 ) ;
#10737 = FACE_OUTER_BOUND ( 'NONE', #2122, .T. ) ;
#10738 = SURFACE_STYLE_FILL_AREA ( #18971 ) ;
#10739 = CARTESIAN_POINT ( 'NONE',  ( 36.80608444377001121, -19.31368208888609672, 70.35351908239857721 ) ) ;
#10740 = DIRECTION ( 'NONE',  ( 2.690219486203388234E-15, -0.8967398287344627850, -0.4425581086832399147 ) ) ;
#10741 = CYLINDRICAL_SURFACE ( 'NONE', #20445, 1.750000000000001554 ) ;
#10742 = EDGE_CURVE ( 'NONE', #19743, #3268, #19895, .T. ) ;
#10743 = ORIENTED_EDGE ( 'NONE', *, *, #12244, .T. ) ;
#10744 = ADVANCED_FACE ( 'NONE', ( #17969 ), #8173, .T. ) ;
#10745 = LINE ( 'NONE', #9921, #19479 ) ;
#10746 = DIRECTION ( 'NONE',  ( -1.000000000000000000, -2.999999999999999839E-15, 0.000000000000000000 ) ) ;
#10747 = ADVANCED_FACE ( 'NONE', ( #12804 ), #18722, .T. ) ;
#10748 = CARTESIAN_POINT ( 'NONE',  ( 37.33957961208645315, -15.80384086642190589, 69.94417936956672577 ) ) ;
#10749 = DIRECTION ( 'NONE',  ( 1.000000000000000000, 0.000000000000000000, 0.000000000000000000 ) ) ;
#10750 = CARTESIAN_POINT ( 'NONE',  ( 33.56477571746443544, 3.418883076854447367, 6.349191931652266696 ) ) ;
#10751 = CARTESIAN_POINT ( 'NONE',  ( 34.81606138205696510, -2.443590368994793760, -5.798199789213649424 ) ) ;
#10752 = CIRCLE ( 'NONE', #14037, 1.500000000000000222 ) ;
#10753 = DIRECTION ( 'NONE',  ( 2.792262043613788535E-15, -0.8967398287344627850, -0.4425581086832399147 ) ) ;
#10754 = CARTESIAN_POINT ( 'NONE',  ( 36.80608444377001831, -26.30384086642191477, 72.40698646996133903 ) ) ;
#10755 = CARTESIAN_POINT ( 'NONE',  ( 38.31606138205700063, -6.758471399387619094, 56.13572720721855092 ) ) ;
#10756 = ORIENTED_EDGE ( 'NONE', *, *, #20283, .T. ) ;
#10757 = ADVANCED_FACE ( 'NONE', ( #24613 ), #5903, .T. ) ;
#10758 = CARTESIAN_POINT ( 'NONE',  ( 38.93415946300897446, -26.11368208888610098, 73.09843995877328382 ) ) ;
#10759 = ORIENTED_EDGE ( 'NONE', *, *, #20936, .T. ) ;
#10760 = ORIENTED_EDGE ( 'NONE', *, *, #199, .F. ) ;
#10761 = CARTESIAN_POINT ( 'NONE',  ( 30.81606138205697931, -6.210967385200574675, -3.065230171572521645 ) ) ;
#10762 = FACE_OUTER_BOUND ( 'NONE', #3191, .T. ) ;
#10763 = CARTESIAN_POINT ( 'NONE',  ( 37.69225076346193504, -1.813682088886100274, 72.33091598616827866 ) ) ;
#10764 = CARTESIAN_POINT ( 'NONE',  ( 37.38336156205274818, 0.2863179111139008137, 72.12822762946751709 ) ) ;
#10765 = VERTEX_POINT ( 'NONE', #2607 ) ;
#10766 = ORIENTED_EDGE ( 'NONE', *, *, #16022, .F. ) ;
#10767 = CARTESIAN_POINT ( 'NONE',  ( 36.31606138205700063, -11.53103574255889185, 17.35070425506816605 ) ) ;
#10768 = PLANE ( 'NONE',  #22352 ) ;
#10769 = ORIENTED_EDGE ( 'NONE', *, *, #14313, .T. ) ;
#10770 = CARTESIAN_POINT ( 'NONE',  ( 37.80618814713138676, -1.703840866421908018, 69.62690120949091011 ) ) ;
#10771 = DIRECTION ( 'NONE',  ( -8.673617379884039170E-17, 1.163336342344340343E-15, -1.000000000000000000 ) ) ;
#10772 = CARTESIAN_POINT ( 'NONE',  ( 39.81606138205700063, -6.758471399387619094, 56.13572720721855092 ) ) ;
#10773 = VERTEX_POINT ( 'NONE', #14471 ) ;
#10774 = ORIENTED_EDGE ( 'NONE', *, *, #23168, .T. ) ;
#10775 = ORIENTED_EDGE ( 'NONE', *, *, #2521, .F. ) ;
#10776 = CARTESIAN_POINT ( 'NONE',  ( 39.98359781491296161, 1.586317911113896528, 71.86517103874049894 ) ) ;
#10777 = CARTESIAN_POINT ( 'NONE',  ( 32.31606138205700063, -20.93319939328399926, 43.78741072286599945 ) ) ;
#10778 = CARTESIAN_POINT ( 'NONE',  ( 46.81606138205705037, -30.46100403034029114, 72.05704881431049103 ) ) ;
#10779 = DIRECTION ( 'NONE',  ( -0.000000000000000000, -0.7540134720837717852, -0.6568589528324747517 ) ) ;
#10780 = LINE ( 'NONE', #24664, #2037 ) ;
#10781 = CARTESIAN_POINT ( 'NONE',  ( 33.31606138205700773, -13.25716901376043033, 21.21736665487721041 ) ) ;
#10782 = EDGE_CURVE ( 'NONE', #6498, #8460, #18268, .T. ) ;
#10783 = AXIS2_PLACEMENT_3D ( 'NONE', #7572, #15286, #3687 ) ;
#10784 = LINE ( 'NONE', #18635, #17333 ) ;
#10785 = ORIENTED_EDGE ( 'NONE', *, *, #6950, .T. ) ;
#10786 = EDGE_LOOP ( 'NONE', ( #15532, #8220, #22506, #25370 ) ) ;
#10787 = CARTESIAN_POINT ( 'NONE',  ( 43.69896204258590444, 3.548173818309678484, 6.215045287937394747 ) ) ;
#10788 = CARTESIAN_POINT ( 'NONE',  ( 36.81465384343994884, 41.67000142393845152, 79.37823623207322044 ) ) ;
#10789 = CARTESIAN_POINT ( 'NONE',  ( 38.73920764526925353, -18.11368208888610098, 72.49843995877330372 ) ) ;
#10790 = ORIENTED_EDGE ( 'NONE', *, *, #8068, .F. ) ;
#10791 = ORIENTED_EDGE ( 'NONE', *, *, #22807, .T. ) ;
#10792 = AXIS2_PLACEMENT_3D ( 'NONE', #7085, #16879, #3084 ) ;
#10793 = DIRECTION ( 'NONE',  ( -1.734723475976814737E-16, 0.000000000000000000, -1.000000000000000000 ) ) ;
#10794 = CARTESIAN_POINT ( 'NONE',  ( 38.37017380507020192, -0.01368208888610777940, 73.11602215082118050 ) ) ;
#10795 = CARTESIAN_POINT ( 'NONE',  ( 39.95015449827720744, -21.00384086642191406, 71.96809898377887293 ) ) ;
#10796 = CARTESIAN_POINT ( 'NONE',  ( 36.31606138205700063, -29.06829118875199924, 75.80501292737000085 ) ) ;
#10797 = CARTESIAN_POINT ( 'NONE',  ( 36.89935272106204422, -11.21368208888610241, 69.52238214136768590 ) ) ;
#10798 = DIRECTION ( 'NONE',  ( -1.734723475976804876E-16, -3.430248998885765387E-15, -1.000000000000000000 ) ) ;
#10799 = CARTESIAN_POINT ( 'NONE',  ( 33.23058527440272059, 3.113468987225112006, 6.136968036621317069 ) ) ;
#10800 = CARTESIAN_POINT ( 'NONE',  ( 33.24019963865212191, 3.104051971978903701, 6.135536383744724098 ) ) ;
#10801 = AXIS2_PLACEMENT_3D ( 'NONE', #996, #10934, #1388 ) ;
#10802 = CARTESIAN_POINT ( 'NONE',  ( 31.81606138205700418, 38.19123852234599070, 73.05501292736988717 ) ) ;
#10803 = CARTESIAN_POINT ( 'NONE',  ( 40.56606138205695800, 0.3291273985901211896, 13.05748091128652533 ) ) ;
#10804 = LINE ( 'NONE', #8750, #2771 ) ;
#10805 = CIRCLE ( 'NONE', #19851, 2.500000000000002220 ) ;
#10806 = DIRECTION ( 'NONE',  ( 2.782607932743246094E-15, -0.8967398287344627850, -0.4425581086832399147 ) ) ;
#10807 = ORIENTED_EDGE ( 'NONE', *, *, #16571, .T. ) ;
#10808 = CARTESIAN_POINT ( 'NONE',  ( 43.81606138205700063, 41.44123852234599070, 73.55501292736987295 ) ) ;
#10809 = VECTOR ( 'NONE', #22013, 1000.000000000000000 ) ;
#10810 = EDGE_CURVE ( 'NONE', #17954, #1877, #8933, .T. ) ;
#10811 = CARTESIAN_POINT ( 'NONE',  ( 33.03722820848892638, 1.142818861812999742, 82.55501292736998664 ) ) ;
#10812 = ORIENTED_EDGE ( 'NONE', *, *, #5948, .T. ) ;
#10813 = EDGE_LOOP ( 'NONE', ( #21247, #3269, #20325, #12543 ) ) ;
#10814 = UNCERTAINTY_MEASURE_WITH_UNIT (LENGTH_MEASURE( 1.000000000000000082E-05 ), #24666, 'distance_accuracy_value', 'NONE');
#10815 = CARTESIAN_POINT ( 'NONE',  ( 40.52078840805429394, -19.00384086642191406, 72.15350918040381600 ) ) ;
#10816 = AXIS2_PLACEMENT_3D ( 'NONE', #24257, #6128, #22215 ) ;
#10817 = CARTESIAN_POINT ( 'NONE',  ( 38.26194895904383486, -23.01368208888609956, 69.64448340153877837 ) ) ;
#10818 = CARTESIAN_POINT ( 'NONE',  ( 40.81606138205700773, -24.05876147765400219, 74.30501292737008612 ) ) ;
#10819 = VECTOR ( 'NONE', #18007, 1000.000000000000227 ) ;
#10820 = DIRECTION ( 'NONE',  ( -1.000000000000000000, -1.052872940142565459E-15, -1.848188032574765003E-17 ) ) ;
#10821 = ORIENTED_EDGE ( 'NONE', *, *, #6900, .T. ) ;
#10822 = CARTESIAN_POINT ( 'NONE',  ( 33.31606138205700773, -2.088476903695762665, 19.19551655256602984 ) ) ;
#10823 = DIRECTION ( 'NONE',  ( -1.000000000000000078E-15, 0.9439899321577400748, 0.3299742535180970049 ) ) ;
#10824 = VECTOR ( 'NONE', #12040, 1000.000000000000000 ) ;
#10825 = CARTESIAN_POINT ( 'NONE',  ( 40.26954217208371034, -26.71368208888610596, 69.89063713639254161 ) ) ;
#10826 = ORIENTED_EDGE ( 'NONE', *, *, #458, .F. ) ;
#10827 = EDGE_CURVE ( 'NONE', #23038, #25254, #16269, .T. ) ;
#10828 = LINE ( 'NONE', #17008, #1173 ) ;
#10829 = DIRECTION ( 'NONE',  ( -2.690219486203388234E-15, 0.8967398287344627850, 0.4425581086832399147 ) ) ;
#10830 = CARTESIAN_POINT ( 'NONE',  ( 39.82603832034400426, -4.313682088886107380, 72.40698646996135324 ) ) ;
#10831 = DIRECTION ( 'NONE',  ( -2.515133600231165483E-15, 0.7516416929448815898, 0.6595716529892353686 ) ) ;
#10832 = ADVANCED_FACE ( 'NONE', ( #669 ), #8556, .F. ) ;
#10833 = VECTOR ( 'NONE', #12995, 1000.000000000000114 ) ;
#10834 = CARTESIAN_POINT ( 'NONE',  ( 39.75915168707250302, -22.71368208888610241, 70.26145752964252722 ) ) ;
#10835 = ADVANCED_FACE ( 'NONE', ( #800 ), #2987, .F. ) ;
#10836 = ADVANCED_FACE ( 'NONE', ( #16391 ), #20786, .F. ) ;
#10837 = EDGE_CURVE ( 'NONE', #11585, #22327, #9210, .T. ) ;
#10838 = CARTESIAN_POINT ( 'NONE',  ( 38.58006293444520196, -22.20876388569947935, 75.80498974974848636 ) ) ;
#10839 = AXIS2_PLACEMENT_3D ( 'NONE', #23222, #10341, #4549 ) ;
#10840 = DIRECTION ( 'NONE',  ( -1.000000000000000000, 0.000000000000000000, 1.586291242107190025E-15 ) ) ;
#10841 = CARTESIAN_POINT ( 'NONE',  ( 38.00113996487112189, -19.70384086642190979, 70.22690120949090442 ) ) ;
#10842 = CARTESIAN_POINT ( 'NONE',  ( 38.26194895904383486, -7.013682088886100452, 69.64448340153879258 ) ) ;
#10843 = CARTESIAN_POINT ( 'NONE',  ( 31.81606138205700418, -26.74044063519535186, 82.50501292737007475 ) ) ;
#10844 = CIRCLE ( 'NONE', #24393, 0.5000000000000001110 ) ;
#10845 = EDGE_CURVE ( 'NONE', #16878, #8203, #16781, .T. ) ;
#10846 = VERTEX_POINT ( 'NONE', #8687 ) ;
#10847 = ADVANCED_FACE ( 'NONE', ( #14845 ), #22703, .T. ) ;
#10848 = CARTESIAN_POINT ( 'NONE',  ( 37.25202387243754032, -4.403840866421916189, 72.75271321436733274 ) ) ;
#10849 = DIRECTION ( 'NONE',  ( -1.000000000000000000, 0.000000000000000000, 0.000000000000000000 ) ) ;
#10850 = VECTOR ( 'NONE', #15772, 1000.000000000000000 ) ;
#10851 = CARTESIAN_POINT ( 'NONE',  ( 39.82603832034400426, -6.313682088886107380, 72.40698646996135324 ) ) ;
#10852 = ORIENTED_EDGE ( 'NONE', *, *, #23357, .T. ) ;
#10853 = CARTESIAN_POINT ( 'NONE',  ( 40.33642880535524000, -12.31368208888611093, 72.77780686321126780 ) ) ;
#10854 = VERTEX_POINT ( 'NONE', #10490 ) ;
#10855 = CARTESIAN_POINT ( 'NONE',  ( 36.31606138205700063, -5.204193249396356968, 72.80501292736992980 ) ) ;
#10856 = CARTESIAN_POINT ( 'NONE',  ( 38.93987200065210175, -12.80384086642190944, 72.33091598616826445 ) ) ;
#10857 = CARTESIAN_POINT ( 'NONE',  ( 31.81606138205700418, 41.44123852234599781, 75.30501292736988717 ) ) ;
#10858 = EDGE_CURVE ( 'NONE', #1424, #13483, #14346, .T. ) ;
#10859 = ORIENTED_EDGE ( 'NONE', *, *, #7939, .F. ) ;
#10860 = CYLINDRICAL_SURFACE ( 'NONE', #13781, 0.7500000000000006661 ) ;
#10861 = LINE ( 'NONE', #3234, #17023 ) ;
#10862 = CARTESIAN_POINT ( 'NONE',  ( 36.89935272106205133, -16.40384086642191974, 73.23812341099225875 ) ) ;
#10863 = VECTOR ( 'NONE', #12399, 1000.000000000000227 ) ;
#10864 = DIRECTION ( 'NONE',  ( 1.734723475976804876E-16, -1.163336342344340343E-15, 1.000000000000000000 ) ) ;
#10865 = LINE ( 'NONE', #20781, #12440 ) ;
#10866 = CARTESIAN_POINT ( 'NONE',  ( 36.49096545463212493, -17.51368208888610667, 71.43714994484034264 ) ) ;
#10867 = FACE_OUTER_BOUND ( 'NONE', #3351, .T. ) ;
#10868 = CIRCLE ( 'NONE', #15377, 1.750000000000001554 ) ;
#10869 = LINE ( 'NONE', #10612, #14320 ) ;
#10870 = ORIENTED_EDGE ( 'NONE', *, *, #11241, .F. ) ;
#10871 = DIRECTION ( 'NONE',  ( 0.000000000000000000, -3.491481338843135327E-15, -1.000000000000000000 ) ) ;
#10872 = DIRECTION ( 'NONE',  ( 6.489379976170840313E-31, -1.000000000000000000, 3.491481338843135327E-15 ) ) ;
#10873 = CARTESIAN_POINT ( 'NONE',  ( 38.37017380507018771, -13.60384086642190837, 69.64448340153877837 ) ) ;
#10874 = CARTESIAN_POINT ( 'NONE',  ( 33.57054761034910229, 3.412271088041349820, 6.349711998884802533 ) ) ;
#10875 = CARTESIAN_POINT ( 'NONE',  ( 36.68196826583682935, -25.61368208888610454, 71.96809898377887293 ) ) ;
#10876 = CARTESIAN_POINT ( 'NONE',  ( 32.81606138205700773, 28.12806996228107081, 65.30501292736992980 ) ) ;
#10877 = VECTOR ( 'NONE', #16932, 1000.000000000000000 ) ;
#10878 = CARTESIAN_POINT ( 'NONE',  ( 38.93415946300896024, -23.50384086642189985, 69.66206559358661821 ) ) ;
#10879 = CARTESIAN_POINT ( 'NONE',  ( 36.51558096900348005, -21.15780082040966903, 75.86401592669550098 ) ) ;
#10880 = CARTESIAN_POINT ( 'NONE',  ( 36.87297107704152666, -23.71368208888610951, 72.49904802271738902 ) ) ;
#10881 = ORIENTED_EDGE ( 'NONE', *, *, #22395, .F. ) ;
#10882 = ORIENTED_EDGE ( 'NONE', *, *, #3161, .F. ) ;
#10883 = CARTESIAN_POINT ( 'NONE',  ( 34.81606138205700773, -21.26162886970023536, 44.16441745890789150 ) ) ;
#10884 = PLANE ( 'NONE',  #3049 ) ;
#10885 = CARTESIAN_POINT ( 'NONE',  ( 38.37017380507018771, -29.60384086642191193, 70.24448340153875847 ) ) ;
#10886 = CARTESIAN_POINT ( 'NONE',  ( 37.25260217561390874, 0.3863179111139002364, 71.78268878715394408 ) ) ;
#10887 = VERTEX_POINT ( 'NONE', #20270 ) ;
#10888 = EDGE_CURVE ( 'NONE', #6498, #22104, #24367, .T. ) ;
#10889 = ORIENTED_EDGE ( 'NONE', *, *, #18763, .F. ) ;
#10890 = CARTESIAN_POINT ( 'NONE',  ( 43.81606138205700063, 3.913963181809303027, 6.295759124378626836 ) ) ;
#10891 = DIRECTION ( 'NONE',  ( -1.000000000000000000, 4.930380657631319405E-32, 1.734723475976804876E-16 ) ) ;
#10892 = VERTEX_POINT ( 'NONE', #6744 ) ;
#10893 = CARTESIAN_POINT ( 'NONE',  ( 39.98359781491296161, -5.203840866421911571, 70.89533451361947414 ) ) ;
#10894 = CARTESIAN_POINT ( 'NONE',  ( 43.31606138205700063, -38.37466412126273951, 70.68129701848354784 ) ) ;
#10895 = MECHANICAL_DESIGN_GEOMETRIC_PRESENTATION_REPRESENTATION (  '', ( #9255 ), #172 ) ;
#10896 = CARTESIAN_POINT ( 'NONE',  ( 33.31606138205700773, -13.04008168869995288, 21.66778101221729713 ) ) ;
#10897 = ORIENTED_EDGE ( 'NONE', *, *, #6983, .F. ) ;
#10898 = VECTOR ( 'NONE', #9191, 1000.000000000000000 ) ;
#10899 = ORIENTED_EDGE ( 'NONE', *, *, #9857, .F. ) ;
#10900 = EDGE_LOOP ( 'NONE', ( #21455, #23238, #1569, #20821, #12695, #19741, #21236, #24698 ) ) ;
#10901 = PLANE ( 'NONE',  #1760 ) ;
#10902 = CARTESIAN_POINT ( 'NONE',  ( 38.93415946300898867, -2.113682088886109423, 73.09843995877331224 ) ) ;
#10903 = ORIENTED_EDGE ( 'NONE', *, *, #9895, .T. ) ;
#10904 = DIRECTION ( 'NONE',  ( 0.000000000000000000, 0.8967398287344627850, 0.4425581086832398037 ) ) ;
#10905 = VECTOR ( 'NONE', #9197, 1000.000000000000000 ) ;
#10906 = FACE_OUTER_BOUND ( 'NONE', #23813, .T. ) ;
#10907 = DIRECTION ( 'NONE',  ( -9.925461516413219746E-16, 0.8967398287344630070, 0.4425581086832393041 ) ) ;
#10908 = LINE ( 'NONE', #10299, #18687 ) ;
#10909 = DIRECTION ( 'NONE',  ( -1.000000000000000000, -1.734723475976804876E-16, 1.734723475976814737E-16 ) ) ;
#10910 = CARTESIAN_POINT ( 'NONE',  ( 36.73573221557511204, -5.934306775458773053, 82.77886294573366399 ) ) ;
#10911 =( LENGTH_UNIT ( ) NAMED_UNIT ( * ) SI_UNIT ( .MILLI., .METRE. ) );
#10912 = PLANE ( 'NONE',  #11573 ) ;
#10913 = ORIENTED_EDGE ( 'NONE', *, *, #4063, .T. ) ;
#10914 = ORIENTED_EDGE ( 'NONE', *, *, #19001, .F. ) ;
#10915 = CIRCLE ( 'NONE', #16684, 0.7500000000000006661 ) ;
#10917 = ADVANCED_FACE ( 'NONE', ( #24238 ), #6611, .T. ) ;
#10916 = DIRECTION ( 'NONE',  ( -1.000000000000000000, 0.000000000000000000, 0.000000000000000000 ) ) ;
#10918 = CARTESIAN_POINT ( 'NONE',  ( 34.06606138205700773, -40.62725863591898445, 68.52362519861142687 ) ) ;
#10919 = EDGE_CURVE ( 'NONE', #16707, #10709, #10745, .T. ) ;
#10920 = CARTESIAN_POINT ( 'NONE',  ( 37.60469502381300089, -19.21368208888609885, 70.49320253461759478 ) ) ;
#10921 = ORIENTED_EDGE ( 'NONE', *, *, #18708, .F. ) ;
#10922 = ORIENTED_EDGE ( 'NONE', *, *, #8766, .F. ) ;
#10923 = CARTESIAN_POINT ( 'NONE',  ( 29.81606138205696155, -0.2703287878658162113, 1.505452687840413972 ) ) ;
#10924 = ORIENTED_EDGE ( 'NONE', *, *, #5117, .F. ) ;
#10925 = CARTESIAN_POINT ( 'NONE',  ( 39.82603832034400426, -2.313682088886107380, 72.40698646996135324 ) ) ;
#10926 = CARTESIAN_POINT ( 'NONE',  ( 36.64852494920107517, -26.20384086642191335, 71.86517103874047052 ) ) ;
#10927 = PLANE ( 'NONE',  #23138 ) ;
#10928 = CARTESIAN_POINT ( 'NONE',  ( 40.26954217208371034, -10.71368208888610063, 69.89063713639259845 ) ) ;
#10929 = CYLINDRICAL_SURFACE ( 'NONE', #1006, 1.000000000000000888 ) ;
#10930 = CARTESIAN_POINT ( 'NONE',  ( 43.81606138205700063, 39.55420052130484265, 58.58767820587064534 ) ) ;
#10931 = ADVANCED_FACE ( 'NONE', ( #20910 ), #25347, .F. ) ;
#10932 = LINE ( 'NONE', #4746, #17602 ) ;
#10933 = VECTOR ( 'NONE', #17380, 1000.000000000000000 ) ;
#10934 = DIRECTION ( 'NONE',  ( -1.000000000000000000, -2.168404344971005170E-16, 1.734723475976814737E-16 ) ) ;
#10935 = CARTESIAN_POINT ( 'NONE',  ( 40.11623881305710881, -6.269741973556977044, 82.74875808203118766 ) ) ;
#10936 = CARTESIAN_POINT ( 'NONE',  ( 31.81606138205700418, 38.19123852234598360, 71.05501292736988717 ) ) ;
#10937 = DIRECTION ( 'NONE',  ( -1.000000000000000000, -3.087130386257447501E-15, -3.221081844416023957E-17 ) ) ;
#10938 = VERTEX_POINT ( 'NONE', #1783 ) ;
#10939 = LINE ( 'NONE', #16990, #16443 ) ;
#10940 = DIRECTION ( 'NONE',  ( -1.734723475976804876E-16, -3.491481338843135327E-15, -1.000000000000000000 ) ) ;
#10941 = ORIENTED_EDGE ( 'NONE', *, *, #1650, .F. ) ;
#10942 = ORIENTED_EDGE ( 'NONE', *, *, #14483, .F. ) ;
#10943 = CARTESIAN_POINT ( 'NONE',  ( 40.55423172469004101, -19.20384086642191335, 70.70992431699450265 ) ) ;
#10944 = CARTESIAN_POINT ( 'NONE',  ( 39.75915168707250302, -22.71368208888610241, 70.26145752964251301 ) ) ;
#10945 = PLANE ( 'NONE',  #4149 ) ;
#10946 = CARTESIAN_POINT ( 'NONE',  ( 43.31606138205700063, -22.22127907754186893, 75.80501292736997243 ) ) ;
#10947 = ORIENTED_EDGE ( 'NONE', *, *, #19973, .T. ) ;
#10948 = DIRECTION ( 'NONE',  ( 1.202852874072920494E-15, -0.3934158747763039088, 0.9193606199277819524 ) ) ;
#10949 = DIRECTION ( 'NONE',  ( 9.999999999999998805E-16, -0.9439899321577399638, -0.3299742535180969494 ) ) ;
#10950 = CARTESIAN_POINT ( 'NONE',  ( 38.37017380507018771, 0.3961591335780896284, 69.04448340153882668 ) ) ;
#10951 = ORIENTED_EDGE ( 'NONE', *, *, #25045, .T. ) ;
#10952 = FACE_OUTER_BOUND ( 'NONE', #10122, .T. ) ;
#10953 = APPLICATION_CONTEXT ( 'automotive_design' ) ;
#10954 = DIRECTION ( 'NONE',  ( 1.000000000000000000, -1.301042606982604506E-30, -4.336808689942015271E-16 ) ) ;
#10955 = CARTESIAN_POINT ( 'NONE',  ( 38.26194895904383486, -1.013682088886101784, 69.64448340153879258 ) ) ;
#10956 = CARTESIAN_POINT ( 'NONE',  ( 36.31606138205700063, -11.51539968388052060, 18.41550321377400934 ) ) ;
#10957 = EDGE_CURVE ( 'NONE', #5909, #23734, #17048, .T. ) ;
#10958 = CARTESIAN_POINT ( 'NONE',  ( 39.38009889167650357, -22.21368208888610951, 72.75271321436731853 ) ) ;
#10959 = DIRECTION ( 'NONE',  ( 1.000000000000000000, 0.000000000000000000, 0.000000000000000000 ) ) ;
#10960 = DIRECTION ( 'NONE',  ( -1.000000000000000000, -1.518641380243644581E-16, -1.055262346480601087E-16 ) ) ;
#10961 = CARTESIAN_POINT ( 'NONE',  ( 38.63098279924290068, -18.70384086642191335, 72.53360434286904024 ) ) ;
#10962 = CARTESIAN_POINT ( 'NONE',  ( 37.25202387243752611, -3.213682088886102406, 70.00779233799264034 ) ) ;
#10963 = VERTEX_POINT ( 'NONE', #22959 ) ;
#10964 = CARTESIAN_POINT ( 'NONE',  ( 40.31606138205701484, -20.48435987709931183, 75.45335281290067542 ) ) ;
#10965 = ORIENTED_EDGE ( 'NONE', *, *, #15849, .F. ) ;
#10966 = CARTESIAN_POINT ( 'NONE',  ( 36.87297107704149823, -5.903840866421907307, 70.26145752964255564 ) ) ;
#10967 = EDGE_CURVE ( 'NONE', #13165, #14979, #21633, .T. ) ;
#10968 = DIRECTION ( 'NONE',  ( -1.734723475976814737E-16, 0.000000000000000000, -1.000000000000000000 ) ) ;
#10969 = ADVANCED_FACE ( 'NONE', ( #13185 ), #24875, .T. ) ;
#10970 = CARTESIAN_POINT ( 'NONE',  ( 37.25202387243752611, -3.213682088886102406, 70.00779233799264034 ) ) ;
#10971 = EDGE_LOOP ( 'NONE', ( #3912, #10436, #23478, #5214 ) ) ;
#10972 = CARTESIAN_POINT ( 'NONE',  ( 36.89935272106204422, -7.213682088886102406, 69.52238214136768590 ) ) ;
#10973 = EDGE_LOOP ( 'NONE', ( #18626, #21487, #6501, #17423 ) ) ;
#10974 = DIRECTION ( 'NONE',  ( -1.000000000000000000, 0.000000000000000000, 0.000000000000000000 ) ) ;
#10975 = EDGE_CURVE ( 'NONE', #10597, #17161, #19436, .T. ) ;
#10976 = CARTESIAN_POINT ( 'NONE',  ( 38.37017380507018771, -13.60384086642191193, 70.24448340153875847 ) ) ;
#10977 = EDGE_CURVE ( 'NONE', #24693, #24906, #13054, .T. ) ;
#10978 = CARTESIAN_POINT ( 'NONE',  ( 30.81606138205706813, -36.31746077171918330, 73.86860304758450013 ) ) ;
#10979 = ORIENTED_EDGE ( 'NONE', *, *, #14426, .T. ) ;
#10980 = PLANE ( 'NONE',  #3897 ) ;
#10981 = CARTESIAN_POINT ( 'NONE',  ( 40.31606138205700773, -5.204193249396356968, 72.80501292736992980 ) ) ;
#10982 = CARTESIAN_POINT ( 'NONE',  ( 40.55423172469004101, -19.20384086642191335, 70.70992431699450265 ) ) ;
#10983 = SHAPE_REPRESENTATION ( 'Anvil Plate', ( #2000 ), #16613 ) ;
#10984 = CARTESIAN_POINT ( 'NONE',  ( 36.37840728046802496, -20.73258112307092915, 75.41050264957048910 ) ) ;
#10985 = SURFACE_STYLE_USAGE ( .BOTH. , #23073 ) ;
#10986 = CARTESIAN_POINT ( 'NONE',  ( 40.14115730948191185, -20.51368208888609601, 71.32335560751960202 ) ) ;
#10987 = CYLINDRICAL_SURFACE ( 'NONE', #16648, 3.999999999999999556 ) ;
#10988 = ADVANCED_FACE ( 'NONE', ( #5922 ), #7862, .T. ) ;
#10989 = DIRECTION ( 'NONE',  ( 3.717264591378870232E-16, 3.129456975819164530E-15, 1.000000000000000000 ) ) ;
#10990 = VERTEX_POINT ( 'NONE', #3244 ) ;
#10991 = CARTESIAN_POINT ( 'NONE',  ( 36.31606138205700773, -21.38339321089542722, 27.67811916372966863 ) ) ;
#10992 = CARTESIAN_POINT ( 'NONE',  ( 39.98359781491296161, -11.20384086642191335, 70.89533451361947414 ) ) ;
#10993 = CIRCLE ( 'NONE', #14279, 4.000000000000000000 ) ;
#10994 = DIRECTION ( 'NONE',  ( 0.000000000000000000, 0.000000000000000000, 1.000000000000000000 ) ) ;
#10995 = LINE ( 'NONE', #5072, #3002 ) ;
#10996 = CARTESIAN_POINT ( 'NONE',  ( 36.87297107704152666, -25.71368208888609885, 72.49904802271738902 ) ) ;
#10997 = VECTOR ( 'NONE', #22070, 1000.000000000000227 ) ;
#10998 = VECTOR ( 'NONE', #20630, 1000.000000000000000 ) ;
#10999 = DIRECTION ( 'NONE',  ( 0.000000000000000000, 1.000000000000000000, -1.387778780781444413E-14 ) ) ;
#11000 = CARTESIAN_POINT ( 'NONE',  ( 37.25202387243754032, -22.40384086642191619, 72.75271321436731853 ) ) ;
#11001 = CARTESIAN_POINT ( 'NONE',  ( 36.99021717747880444, -21.74921351108408984, 75.81633765512088985 ) ) ;
#11002 = CARTESIAN_POINT ( 'NONE',  ( 37.25202387243752611, -25.21368208888610241, 70.00779233799262613 ) ) ;
#11003 = ORIENTED_EDGE ( 'NONE', *, *, #6350, .F. ) ;
#11004 = ORIENTED_EDGE ( 'NONE', *, *, #24176, .F. ) ;
#11005 = CARTESIAN_POINT ( 'NONE',  ( 32.81606138205700773, -27.25871422114667553, 59.79942265548595515 ) ) ;
#11006 = CARTESIAN_POINT ( 'NONE',  ( 43.31606138205700773, -18.80550481115970740, 25.27912300651437150 ) ) ;
#11007 = CARTESIAN_POINT ( 'NONE',  ( 37.60469502381300089, 0.7863179111138978161, 70.49320253461759478 ) ) ;
#11008 = EDGE_CURVE ( 'NONE', #1424, #1244, #1390, .T. ) ;
#11009 = EDGE_CURVE ( 'NONE', #25398, #9965, #23600, .T. ) ;
#11010 = ORIENTED_EDGE ( 'NONE', *, *, #2233, .F. ) ;
#11011 = ORIENTED_EDGE ( 'NONE', *, *, #1451, .F. ) ;
#11012 = LINE ( 'NONE', #24891, #986 ) ;
#11013 = LINE ( 'NONE', #20932, #23148 ) ;
#11014 = ORIENTED_EDGE ( 'NONE', *, *, #10532, .T. ) ;
#11015 = DIRECTION ( 'NONE',  ( 1.000000000000000000, 2.999999999999999839E-15, 0.000000000000000000 ) ) ;
#11016 = CARTESIAN_POINT ( 'NONE',  ( 39.29254315202757653, -6.803840866421915656, 72.81632618279323310 ) ) ;
#11017 = CLOSED_SHELL ( 'NONE', ( #20338, #1377, #23533, #6727, #10969, #2684, #9734, #9619, #17436, #19186, #16900, #17073, #19003, #17284, #12114, #13191, #21770, #1525, #2546, #22117, #5174, #12541, #1491, #12268, #12574, #5304, #8235, #3558, #15392, #7556, #8494, #9954, #2163, #4376, #10696, #9034, #12559, #15704, #11399, #15297, #8477, #16224, #7276, #16821, #420, #22963, #11774, #6740, #23807, #15011, #18437, #2544, #8751, #3461, #22288, #11806, #16975, #6578, #22142, #17238, #6426, #22188, #19459, #8942, #9874, #12808, #16226, #252, #17740, #12514, #10747, #11535, #23278, #19179, #13373 ) ) ;
#11018 = DIRECTION ( 'NONE',  ( -0.000000000000000000, -0.8212051873014210024, -0.5706330172266920187 ) ) ;
#11019 = ADVANCED_FACE ( 'NONE', ( #6047 ), #5791, .F. ) ;
#11020 = DIRECTION ( 'NONE',  ( -2.254925078834644814E-15, 0.7516416929448815898, 0.6595716529892353686 ) ) ;
#11021 = ORIENTED_EDGE ( 'NONE', *, *, #1667, .F. ) ;
#11022 = ORIENTED_EDGE ( 'NONE', *, *, #1859, .T. ) ;
#11023 = CARTESIAN_POINT ( 'NONE',  ( 47.84183937708599643, -36.05761098950961241, 70.36375082663613512 ) ) ;
#11024 = CARTESIAN_POINT ( 'NONE',  ( 39.98359781491296161, -0.4136820888861053591, 71.86517103874048473 ) ) ;
#11025 = CARTESIAN_POINT ( 'NONE',  ( 37.69796330110505522, -26.50384086642191050, 73.09843995877328382 ) ) ;
#11026 =( LENGTH_UNIT ( ) NAMED_UNIT ( * ) SI_UNIT ( .MILLI., .METRE. ) );
#11027 = LINE ( 'NONE', #3028, #10420 ) ;
#11028 = ORIENTED_EDGE ( 'NONE', *, *, #8487, .F. ) ;
#11029 = LINE ( 'NONE', #14761, #4475 ) ;
#11030 = EDGE_CURVE ( 'NONE', #2254, #13002, #11288, .T. ) ;
#11031 = CARTESIAN_POINT ( 'NONE',  ( 40.31606138205700773, -22.22127907754180853, 85.30501292736998664 ) ) ;
#11032 = AXIS2_PLACEMENT_3D ( 'NONE', #2812, #18673, #16604 ) ;
#11033 = CARTESIAN_POINT ( 'NONE',  ( 43.31606138205700063, -14.32738121993773994, 11.12118157620986558 ) ) ;
#11034 = DIRECTION ( 'NONE',  ( 0.000000000000000000, 1.000000000000000000, -2.999999999999999839E-15 ) ) ;
#11035 = PRESENTATION_STYLE_ASSIGNMENT (( #15273 ) ) ;
#11036 = AXIS2_PLACEMENT_3D ( 'NONE', #16857, #8270, #13125 ) ;
#11037 = CARTESIAN_POINT ( 'NONE',  ( 45.81606138205700063, 34.87886987267150118, 80.75501292736991843 ) ) ;
#11038 = ORIENTED_EDGE ( 'NONE', *, *, #14749, .T. ) ;
#11039 = ORIENTED_EDGE ( 'NONE', *, *, #4868, .F. ) ;
#11040 = CARTESIAN_POINT ( 'NONE',  ( 35.31606138205687273, 43.19123852234596939, 65.30501292736988717 ) ) ;
#11041 = CARTESIAN_POINT ( 'NONE',  ( 43.06606138205700063, -34.55876147765400930, 73.55501292737011454 ) ) ;
#11042 = CARTESIAN_POINT ( 'NONE',  ( 39.31564783533280405, -14.31368208888609850, 72.03616607671141026 ) ) ;
#11043 = ORIENTED_EDGE ( 'NONE', *, *, #8385, .F. ) ;
#11044 = ORIENTED_EDGE ( 'NONE', *, *, #23565, .F. ) ;
#11045 = CARTESIAN_POINT ( 'NONE',  ( 40.31606138205700773, -21.90577604921433519, 28.73660501626934050 ) ) ;
#11046 = CARTESIAN_POINT ( 'NONE',  ( 38.93415946300897446, -4.113682088886107202, 73.09843995877331224 ) ) ;
#11047 = CARTESIAN_POINT ( 'NONE',  ( 39.82603832034400426, -21.30384086642191122, 70.35351908239857721 ) ) ;
#11048 = LINE ( 'NONE', #10796, #19858 ) ;
#11049 = CARTESIAN_POINT ( 'NONE',  ( 37.50301148336529167, 0.8863179111139005695, 69.06206559358666652 ) ) ;
#11050 = LINE ( 'NONE', #9134, #23221 ) ;
#11051 = ORIENTED_EDGE ( 'NONE', *, *, #12598, .T. ) ;
#11052 = VECTOR ( 'NONE', #20948, 1000.000000000000000 ) ;
#11053 = CARTESIAN_POINT ( 'NONE',  ( 40.25357836725066818, -6.691594714027675472, 83.19992197100876297 ) ) ;
#11054 = CARTESIAN_POINT ( 'NONE',  ( 40.31606138205700773, -5.204193249396356968, 72.80501292736992980 ) ) ;
#11055 = ADVANCED_FACE ( 'NONE', ( #13653 ), #15792, .F. ) ;
#11056 = AXIS2_PLACEMENT_3D ( 'NONE', #6428, #8365, #8104 ) ;
#11057 = DIRECTION ( 'NONE',  ( 2.602085213965210642E-15, -0.8967398287344635621, -0.4425581086832386379 ) ) ;
#11058 = ADVANCED_FACE ( 'NONE', ( #3378 ), #15100, .F. ) ;
#11059 = CARTESIAN_POINT ( 'NONE',  ( 33.56606138205700773, -38.55876147765400930, 73.55501292737012875 ) ) ;
#11060 = DIRECTION ( 'NONE',  ( 0.000000000000000000, 1.000000000000000000, -2.999999999999999839E-15 ) ) ;
#11061 = ADVANCED_FACE ( 'NONE', ( #9202 ), #21037, .F. ) ;
#11062 = VECTOR ( 'NONE', #11912, 1000.000000000000000 ) ;
#11063 = DIRECTION ( 'NONE',  ( -1.327674326049719602E-15, 0.4425581086832399147, -0.8967398287344627850 ) ) ;
#11064 = ORIENTED_EDGE ( 'NONE', *, *, #6174, .F. ) ;
#11065 = CYLINDRICAL_SURFACE ( 'NONE', #9885, 0.7500000000000006661 ) ;
#11066 = DIRECTION ( 'NONE',  ( -1.849283715844614702E-16, 0.8212051873014210024, 0.5706330172266920187 ) ) ;
#11067 = EDGE_LOOP ( 'NONE', ( #13119, #5974, #15699, #7040 ) ) ;
#11068 = ORIENTED_EDGE ( 'NONE', *, *, #15109, .T. ) ;
#11069 = PRODUCT_DEFINITION_CONTEXT ( 'detailed design', #12622, 'design' ) ;
#11070 = VECTOR ( 'NONE', #22544, 1000.000000000000227 ) ;
#11071 = CARTESIAN_POINT ( 'NONE',  ( 39.64521430340305841, -14.80384086642191832, 73.30173637941818754 ) ) ;
#11072 = CIRCLE ( 'NONE', #14358, 1.500000000000001332 ) ;
#11073 = EDGE_CURVE ( 'NONE', #8863, #7140, #11737, .T. ) ;
#11074 = DIRECTION ( 'NONE',  ( -1.000000000000000000, 6.195440985631514482E-17, 1.836970198721027715E-16 ) ) ;
#11075 = CARTESIAN_POINT ( 'NONE',  ( 40.14115730948191185, -18.51368208888610667, 71.32335560751960202 ) ) ;
#11076 = DIRECTION ( 'NONE',  ( -6.071532165918830747E-16, 1.000000000000000000, -3.491481338843135327E-15 ) ) ;
#11077 = VECTOR ( 'NONE', #4122, 1000.000000000000000 ) ;
#11078 =( LENGTH_UNIT ( ) NAMED_UNIT ( * ) SI_UNIT ( .MILLI., .METRE. ) );
#11079 = ORIENTED_EDGE ( 'NONE', *, *, #13521, .F. ) ;
#11080 = LINE ( 'NONE', #12638, #16660 ) ;
#11081 = LINE ( 'NONE', #10571, #20719 ) ;
#11082 = CARTESIAN_POINT ( 'NONE',  ( 38.37017380507020192, -28.01368208888610667, 73.71602215082113219 ) ) ;
#11083 = EDGE_LOOP ( 'NONE', ( #4764, #21183, #14960, #24914, #23262, #8583, #7480, #24883, #24835, #23101, #16129 ) ) ;
#11084 = CIRCLE ( 'NONE', #6958, 0.7500000000000014433 ) ;
#11085 = DIRECTION ( 'NONE',  ( -1.000000000000000000, 0.000000000000000000, 0.000000000000000000 ) ) ;
#11086 = CARTESIAN_POINT ( 'NONE',  ( 44.06606138205700063, 42.11769259596595560, 81.89079936499673806 ) ) ;
#11087 = CARTESIAN_POINT ( 'NONE',  ( 37.80618814713140097, 0.08631791111389161553, 73.13360434286904876 ) ) ;
#11088 = LINE ( 'NONE', #18810, #23613 ) ;
#11089 = CARTESIAN_POINT ( 'NONE',  ( 37.33957961208646736, -11.81368208888610916, 72.81632618279321889 ) ) ;
#11090 = DIRECTION ( 'NONE',  ( -2.727049986597863807E-15, 0.7516416929448760387, 0.6595716529892418079 ) ) ;
#11091 = DIRECTION ( 'NONE',  ( 0.000000000000000000, 1.000000000000000000, -2.775557561562891351E-15 ) ) ;
#11092 = VECTOR ( 'NONE', #19674, 1000.000000000000000 ) ;
#11093 = CARTESIAN_POINT ( 'NONE',  ( 38.26194895904384197, -20.60384086642191193, 72.51602215082118619 ) ) ;
#11094 = CARTESIAN_POINT ( 'NONE',  ( 38.82593461698262871, -2.913682088886099919, 69.62690120949091011 ) ) ;
#11095 = VERTEX_POINT ( 'NONE', #6307 ) ;
#11096 = CARTESIAN_POINT ( 'NONE',  ( 40.56606138205695089, 4.754708485422523445, 4.090082623941899698 ) ) ;
#11097 = ORIENTED_EDGE ( 'NONE', *, *, #6417, .T. ) ;
#11098 = AXIS2_PLACEMENT_3D ( 'NONE', #19261, #17337, #1721 ) ;
#11099 = CARTESIAN_POINT ( 'NONE',  ( 36.87297107704149823, -3.903840866421907752, 70.26145752964255564 ) ) ;
#11100 = PLANE ( 'NONE',  #20120 ) ;
#11101 = ADVANCED_FACE ( 'NONE', ( #4368 ), #229, .F. ) ;
#11102 = CARTESIAN_POINT ( 'NONE',  ( 38.26194895904383486, -1.013682088886101784, 69.64448340153879258 ) ) ;
#11103 = ORIENTED_EDGE ( 'NONE', *, *, #22533, .T. ) ;
#11104 = CARTESIAN_POINT ( 'NONE',  ( 40.55423172469004811, -10.41368208888610347, 72.05058123536544201 ) ) ;
#11105 = AXIS2_PLACEMENT_3D ( 'NONE', #6330, #8515, #24200 ) ;
#11106 = VERTEX_POINT ( 'NONE', #738 ) ;
#11107 = DIRECTION ( 'NONE',  ( 1.000000000000000000, -6.018531076210103283E-31, -1.734723475976805122E-16 ) ) ;
#11108 = CARTESIAN_POINT ( 'NONE',  ( 37.21915885897815457, -14.20384086642191335, 71.67976084211552745 ) ) ;
#11109 = CIRCLE ( 'NONE', #14395, 0.5000000000000004441 ) ;
#11110 = DIRECTION ( 'NONE',  ( 1.000000000000000000, 0.000000000000000000, 0.000000000000000000 ) ) ;
#11111 = ORIENTED_EDGE ( 'NONE', *, *, #2955, .T. ) ;
#11112 = DIRECTION ( 'NONE',  ( 0.000000000000000000, -1.000000000000000000, 0.000000000000000000 ) ) ;
#11113 = CARTESIAN_POINT ( 'NONE',  ( 44.06606138205700063, 40.92314894770294842, 83.08534301325974525 ) ) ;
#11114 = CARTESIAN_POINT ( 'NONE',  ( 40.26954217208372455, -14.90384086642191797, 72.86986841596734621 ) ) ;
#11115 = VECTOR ( 'NONE', #16534, 1000.000000000000227 ) ;
#11116 = CARTESIAN_POINT ( 'NONE',  ( 36.37840728046802496, -20.73333253607436788, 75.41549685518693025 ) ) ;
#11117 = CARTESIAN_POINT ( 'NONE',  ( 37.69796330110504101, -19.11368208888610098, 69.66206559358661821 ) ) ;
#11118 = CARTESIAN_POINT ( 'NONE',  ( 33.31606138205700773, -22.22127907754186893, 75.80501292736997243 ) ) ;
#11119 = AXIS2_PLACEMENT_3D ( 'NONE', #8415, #16126, #24221 ) ;
#11120 = CARTESIAN_POINT ( 'NONE',  ( 30.81606138205707168, -36.80651332587435576, 65.82119181171029254 ) ) ;
#11121 = B_SPLINE_CURVE_WITH_KNOTS ( 'NONE', 3,
 ( #10631, #18482, #14612, #816 ),
 .UNSPECIFIED., .F., .F.,
 ( 4, 4 ),
 ( 0.000000000000000000, 1.000000000000000000 ),
 .UNSPECIFIED. ) ;
#11122 = VECTOR ( 'NONE', #20024, 1000.000000000000000 ) ;
#11123 = ORIENTED_EDGE ( 'NONE', *, *, #11073, .F. ) ;
#11124 = DIRECTION ( 'NONE',  ( 0.000000000000000000, -1.000000000000000000, 2.999999999999999839E-15 ) ) ;
#11125 = LINE ( 'NONE', #6862, #15528 ) ;
#11126 = AXIS2_PLACEMENT_3D ( 'NONE', #21404, #15857, #5821 ) ;
#11127 = CARTESIAN_POINT ( 'NONE',  ( 36.87297107704151244, -7.903840866421909084, 70.26145752964255564 ) ) ;
#11128 = FACE_OUTER_BOUND ( 'NONE', #1924, .T. ) ;
#11129 = CARTESIAN_POINT ( 'NONE',  ( 37.33957961208646736, -27.81368208888611093, 72.81632618279320468 ) ) ;
#11130 = DIRECTION ( 'NONE',  ( 0.000000000000000000, 2.999999999999999839E-15, 1.000000000000000000 ) ) ;
#11131 = CARTESIAN_POINT ( 'NONE',  ( 36.87297107704149823, -25.90384086642190908, 70.26145752964251301 ) ) ;
#11132 = DIRECTION ( 'NONE',  ( 1.000000000000000000, 0.000000000000000000, 0.000000000000000000 ) ) ;
#11133 = VECTOR ( 'NONE', #13669, 1000.000000000000000 ) ;
#11134 = EDGE_CURVE ( 'NONE', #20356, #21012, #10554, .T. ) ;
#11135 = CARTESIAN_POINT ( 'NONE',  ( 39.82603832034400426, -18.31368208888610738, 72.40698646996133903 ) ) ;
#11136 = ORIENTED_EDGE ( 'NONE', *, *, #12599, .T. ) ;
#11137 = CARTESIAN_POINT ( 'NONE',  ( 40.77203464402485622, -28.51368208888610667, 71.32335560751960202 ) ) ;
#11138 = VERTEX_POINT ( 'NONE', #8236 ) ;
#11139 = DIRECTION ( 'NONE',  ( 0.000000000000000000, -2.999999999999999839E-15, -1.000000000000000000 ) ) ;
#11140 = DIRECTION ( 'NONE',  ( -1.000000000000000000, -1.734723475976814737E-16, 0.000000000000000000 ) ) ;
#11141 = SHAPE_REPRESENTATION ( 'Leaf Spring', ( #2000 ), #17482 ) ;
#11142 = CARTESIAN_POINT ( 'NONE',  ( 38.63098279924288647, -0.9136820888861024725, 70.22690120949091863 ) ) ;
#11143 = ORIENTED_EDGE ( 'NONE', *, *, #16871, .F. ) ;
#11144 = ORIENTED_EDGE ( 'NONE', *, *, #20763, .T. ) ;
#11145 = DIRECTION ( 'NONE',  ( -1.000000000000000000, 1.115179377413661005E-30, 3.717264591378870232E-16 ) ) ;
#11146 = CYLINDRICAL_SURFACE ( 'NONE', #8367, 0.7499999999999983347 ) ;
#11147 = EDGE_LOOP ( 'NONE', ( #1463, #20570, #19421, #3007 ) ) ;
#11148 = CARTESIAN_POINT ( 'NONE',  ( 36.87297107704149823, -5.903840866421907307, 70.26145752964255564 ) ) ;
#11149 = DIRECTION ( 'NONE',  ( 0.000000000000000000, 0.4425581086832397482, -0.8967398287344626739 ) ) ;
#11150 = DIRECTION ( 'NONE',  ( -1.000000000000000000, -3.046270958365671426E-15, 5.272995181423179347E-17 ) ) ;
#11151 = ORIENTED_EDGE ( 'NONE', *, *, #11326, .F. ) ;
#11152 = EDGE_CURVE ( 'NONE', #131, #3634, #16327, .T. ) ;
#11153 = ORIENTED_EDGE ( 'NONE', *, *, #23732, .F. ) ;
#11154 = DIRECTION ( 'NONE',  ( 0.000000000000000000, 0.1918498038142821827, -0.9814242980364921154 ) ) ;
#11155 = ADVANCED_FACE ( 'NONE', ( #4496 ), #15952, .F. ) ;
#11156 = AXIS2_PLACEMENT_3D ( 'NONE', #10180, #4511, #21903 ) ;
#11157 = CARTESIAN_POINT ( 'NONE',  ( 38.93415946300898867, -4.113682088886107202, 73.09843995877331224 ) ) ;
#11158 = DIRECTION ( 'NONE',  ( 0.000000000000000000, -1.000000000000000000, 2.999999999999999839E-15 ) ) ;
#11159 = EDGE_CURVE ( 'NONE', #16874, #8450, #23931, .T. ) ;
#11160 = CARTESIAN_POINT ( 'NONE',  ( 40.31606138205700773, 37.94123852234599781, 74.30501292736988717 ) ) ;
#11161 = VECTOR ( 'NONE', #22243, 1000.000000000000000 ) ;
#11162 = ADVANCED_FACE ( 'NONE', ( #24304 ), #19957, .F. ) ;
#11163 = ADVANCED_FACE ( 'NONE', ( #12233 ), #14411, .T. ) ;
#11164 = VERTEX_POINT ( 'NONE', #482 ) ;
#11165 = DIRECTION ( 'NONE',  ( 1.000000000000000000, 0.000000000000000000, 0.000000000000000000 ) ) ;
#11166 = CYLINDRICAL_SURFACE ( 'NONE', #14170, 10.00000000000000178 ) ;
#11167 = CARTESIAN_POINT ( 'NONE',  ( 43.81606138205700063, -33.60910547091194900, 60.61426200347987248 ) ) ;
#11168 = DIRECTION ( 'NONE',  ( 1.000000000000000000, 2.999999999999999839E-15, 0.000000000000000000 ) ) ;
#11169 = SURFACE_STYLE_FILL_AREA ( #8859 ) ;
#11170 = EDGE_LOOP ( 'NONE', ( #12803, #2901, #4852, #22813, #17121 ) ) ;
#11171 = EDGE_CURVE ( 'NONE', #22563, #24485, #24175, .T. ) ;
#11172 = CARTESIAN_POINT ( 'NONE',  ( 38.31606138205700063, 0.6124887759231013584, 82.37823623207334833 ) ) ;
#11173 = ORIENTED_EDGE ( 'NONE', *, *, #4516, .F. ) ;
#11174 = ORIENTED_EDGE ( 'NONE', *, *, #14150, .T. ) ;
#11175 = EDGE_CURVE ( 'NONE', #17340, #17183, #19025, .T. ) ;
#11176 = CARTESIAN_POINT ( 'NONE',  ( 30.81606138205700418, 0.3928188618129990761, 80.05501292737000085 ) ) ;
#11177 = CARTESIAN_POINT ( 'NONE',  ( 41.31606138205700063, 3.536347952325769040, 64.10938348997790115 ) ) ;
#11178 = CARTESIAN_POINT ( 'NONE',  ( 38.63098279924288647, -16.91368208888609814, 70.22690120949090442 ) ) ;
#11179 = EDGE_LOOP ( 'NONE', ( #18701, #1083, #20957, #17066 ) ) ;
#11180 = EDGE_LOOP ( 'NONE', ( #20920, #4033, #15905, #6316 ) ) ;
#11181 = LINE ( 'NONE', #12988, #3810 ) ;
#11182 = ORIENTED_EDGE ( 'NONE', *, *, #9884, .F. ) ;
#11183 = CARTESIAN_POINT ( 'NONE',  ( 35.31606138205700773, 8.104266321858618838, 55.82104096753806033 ) ) ;
#11184 = CARTESIAN_POINT ( 'NONE',  ( 39.29254315202757653, -26.80384086642191477, 72.81632618279320468 ) ) ;
#11185 = VECTOR ( 'NONE', #13617, 1000.000000000000000 ) ;
#11186 = CARTESIAN_POINT ( 'NONE',  ( 42.99498874235398205, 2.839582837266055204, 6.102945014747132468 ) ) ;
#11187 = AXIS2_PLACEMENT_3D ( 'NONE', #5191, #5057, #18582 ) ;
#11188 = CARTESIAN_POINT ( 'NONE',  ( 36.29569395875879678, -3.313682088886101607, 69.98269868914869107 ) ) ;
#11189 = ORIENTED_EDGE ( 'NONE', *, *, #5389, .F. ) ;
#11190 = ORIENTED_EDGE ( 'NONE', *, *, #19159, .T. ) ;
#11191 = DIRECTION ( 'NONE',  ( 0.000000000000000000, 1.000000000000000000, 0.000000000000000000 ) ) ;
#11192 = DIRECTION ( 'NONE',  ( 0.000000000000000000, 0.6568589528324747517, -0.7540134720837717852 ) ) ;
#11193 = DIRECTION ( 'NONE',  ( 0.000000000000000000, 0.9814242980364923374, 0.1918498038142812112 ) ) ;
#11194 = EDGE_CURVE ( 'NONE', #24026, #4345, #14033, .T. ) ;
#11195 = LINE ( 'NONE', #9140, #769 ) ;
#11196 = DIRECTION ( 'NONE',  ( -1.000000000000000000, 0.000000000000000000, 0.000000000000000000 ) ) ;
#11197 = CIRCLE ( 'NONE', #13652, 1.500000000000001332 ) ;
#11198 = CARTESIAN_POINT ( 'NONE',  ( 38.31606138205700063, -1.383222575549920119, 62.14461230196212682 ) ) ;
#11199 = VERTEX_POINT ( 'NONE', #20208 ) ;
#11200 = DIRECTION ( 'NONE',  ( 2.452751524064188892E-15, -1.000000000000000000, 0.000000000000000000 ) ) ;
#11201 = AXIS2_PLACEMENT_3D ( 'NONE', #20829, #17222, #14641 ) ;
#11202 = FACE_OUTER_BOUND ( 'NONE', #14217, .T. ) ;
#11203 = ORIENTED_EDGE ( 'NONE', *, *, #13650, .T. ) ;
#11204 = EDGE_LOOP ( 'NONE', ( #19772, #10965, #13766, #190 ) ) ;
#11205 = CARTESIAN_POINT ( 'NONE',  ( 39.02088643472237806, -12.70384086642191690, 73.73360434286898624 ) ) ;
#11206 = DIRECTION ( 'NONE',  ( -2.792262043613788535E-15, 0.8967398287344627850, 0.4425581086832398592 ) ) ;
#11207 = CARTESIAN_POINT ( 'NONE',  ( 36.80608444377001121, -21.31368208888610027, 70.35351908239857721 ) ) ;
#11208 = EDGE_CURVE ( 'NONE', #1002, #10213, #18648, .T. ) ;
#11209 = SURFACE_SIDE_STYLE ('',( #16605 ) ) ;
#11210 = ORIENTED_EDGE ( 'NONE', *, *, #6417, .F. ) ;
#11211 = PLANE ( 'NONE',  #15429 ) ;
#11212 = PRODUCT_DEFINITION ( 'UNKNOWN', '', #997, #18020 ) ;
#11213 = DIRECTION ( 'NONE',  ( -0.1733269559585509378, 0.000000000000000000, -0.9848643390529188135 ) ) ;
#11214 = CARTESIAN_POINT ( 'NONE',  ( 40.33642880535524000, -18.31368208888610383, 72.77780686321126780 ) ) ;
#11215 = ORIENTED_EDGE ( 'NONE', *, *, #4643, .T. ) ;
#11216 = AXIS2_PLACEMENT_3D ( 'NONE', #5634, #13383, #19286 ) ;
#11217 = DIRECTION ( 'NONE',  ( -0.1733269559585509378, 0.000000000000000000, -0.9848643390529188135 ) ) ;
#11218 = CARTESIAN_POINT ( 'NONE',  ( 38.93415946300897446, -2.113682088886109423, 73.09843995877331224 ) ) ;
#11219 = DIRECTION ( 'NONE',  ( 0.000000000000000000, 0.7540134720837717852, 0.6568589528324746407 ) ) ;
#11220 = AXIS2_PLACEMENT_3D ( 'NONE', #2279, #6419, #18385 ) ;
#11221 = CARTESIAN_POINT ( 'NONE',  ( 40.14115730948191185, -16.51368208888610667, 71.32335560751960202 ) ) ;
#11222 = CARTESIAN_POINT ( 'NONE',  ( 39.66066260159681889, -29.10876147764981781, 69.85357445396793707 ) ) ;
#11223 = AXIS2_PLACEMENT_3D ( 'NONE', #13149, #5028, #16746 ) ;
#11224 = LINE ( 'NONE', #22806, #143 ) ;
#11225 = CARTESIAN_POINT ( 'NONE',  ( 37.60469502381300799, -18.40384086642190908, 72.26730301774234988 ) ) ;
#11226 = CARTESIAN_POINT ( 'NONE',  ( 36.68196826583682935, -7.613682088886103649, 71.96809898377890136 ) ) ;
#11227 = ORIENTED_EDGE ( 'NONE', *, *, #5793, .F. ) ;
#11228 = DIRECTION ( 'NONE',  ( -2.727049986597863807E-15, 0.7516416929448760387, 0.6595716529892418079 ) ) ;
#11229 = LINE ( 'NONE', #4573, #4132 ) ;
#11230 = VERTEX_POINT ( 'NONE', #18035 ) ;
#11231 = VERTEX_POINT ( 'NONE', #14280 ) ;
#11232 = CIRCLE ( 'NONE', #15743, 2.000000000000001776 ) ;
#11233 = CARTESIAN_POINT ( 'NONE',  ( 37.25202387243754032, -6.403840866421914413, 72.75271321436733274 ) ) ;
#11234 = LINE ( 'NONE', #1426, #18471 ) ;
#11235 = AXIS2_PLACEMENT_3D ( 'NONE', #2634, #18491, #14122 ) ;
#11236 = CARTESIAN_POINT ( 'NONE',  ( 38.63098279924288647, -28.91368208888610170, 70.22690120949089021 ) ) ;
#11237 = ORIENTED_EDGE ( 'NONE', *, *, #8668, .T. ) ;
#11238 = CARTESIAN_POINT ( 'NONE',  ( 36.11133435605973574, -7.613682088886103649, 72.15350918040385864 ) ) ;
#11239 = EDGE_LOOP ( 'NONE', ( #19146, #8792, #19461, #19501 ) ) ;
#11240 = DIRECTION ( 'NONE',  ( 0.000000000000000000, -1.000000000000000000, 2.999999999999999839E-15 ) ) ;
#11241 = EDGE_CURVE ( 'NONE', #9515, #9404, #22394, .T. ) ;
#11242 = CARTESIAN_POINT ( 'NONE',  ( 37.38336156205273397, -3.903840866421911748, 70.63227792289248441 ) ) ;
#11243 = EDGE_CURVE ( 'NONE', #3300, #25416, #11910, .T. ) ;
#11244 = DIRECTION ( 'NONE',  ( -0.000000000000000000, -0.8212051873014210024, -0.5706330172266920187 ) ) ;
#11245 = ORIENTED_EDGE ( 'NONE', *, *, #5363, .T. ) ;
#11246 = AXIS2_PLACEMENT_3D ( 'NONE', #16816, #20687, #24402 ) ;
#11247 = CARTESIAN_POINT ( 'NONE',  ( 46.81606138205705037, -30.46100403034031245, 72.05704881431053366 ) ) ;
#11248 = DIRECTION ( 'NONE',  ( -1.000000000000000000, -2.999999999999999839E-15, 0.000000000000000000 ) ) ;
#11249 = CARTESIAN_POINT ( 'NONE',  ( 35.86008812008917346, -8.103840866421913702, 71.32335560751961623 ) ) ;
#11250 = CARTESIAN_POINT ( 'NONE',  ( 38.18494427818247061, -22.22127907754186893, 75.80501292736997243 ) ) ;
#11251 =( BOUNDED_CURVE ( )  B_SPLINE_CURVE ( 3, ( #9878, #21464, #21333, #15912 ),
 .UNSPECIFIED., .F., .T. ) 
 B_SPLINE_CURVE_WITH_KNOTS ( ( 4, 4 ),
 ( 4.712388980384689674, 6.283185307179590673 ),
 .UNSPECIFIED. ) 
 CURVE ( )  GEOMETRIC_REPRESENTATION_ITEM ( )  RATIONAL_B_SPLINE_CURVE ( ( 1.000000000000000000, 0.8047378541243649375, 0.8047378541243649375, 1.000000000000000000 ) ) 
 REPRESENTATION_ITEM ( '' )  );
#11252 = CARTESIAN_POINT ( 'NONE',  ( 36.68196826583682935, -23.61368208888610454, 71.96809898377887293 ) ) ;
#11253 = DIRECTION ( 'NONE',  ( 1.000000000000000000, 0.000000000000000000, 0.000000000000000000 ) ) ;
#11254 = CARTESIAN_POINT ( 'NONE',  ( 31.91606138205697363, -4.349482454670880571, -5.142398479549302515 ) ) ;
#11255 = CIRCLE ( 'NONE', #4262, 1.750000000000001554 ) ;
#11256 = ORIENTED_EDGE ( 'NONE', *, *, #25160, .T. ) ;
#11257 = CARTESIAN_POINT ( 'NONE',  ( 33.56606138205700773, 41.44123852234595518, 61.30501292736988006 ) ) ;
#11258 = DIRECTION ( 'NONE',  ( 0.000000000000000000, 1.000000000000000000, -2.999999999999999839E-15 ) ) ;
#11259 = ADVANCED_FACE ( 'NONE', ( #6934 ), #18656, .F. ) ;
#11260 = CARTESIAN_POINT ( 'NONE',  ( 36.49096545463212493, -6.103840866421912814, 71.32335560751963044 ) ) ;
#11261 = PRODUCT_CONTEXT ( 'NONE', #15387, 'mechanical' ) ;
#11262 = CARTESIAN_POINT ( 'NONE',  ( 34.06606138205700773, -32.75315594507191008, 59.38245422252773409 ) ) ;
#11263 = CARTESIAN_POINT ( 'NONE',  ( 39.38009889167650357, -26.21368208888610951, 72.75271321436730432 ) ) ;
#11264 = CARTESIAN_POINT ( 'NONE',  ( 40.31606138205700773, 37.94123852234599070, 73.55501292736988717 ) ) ;
#11265 = VECTOR ( 'NONE', #25028, 1000.000000000000114 ) ;
#11266 = CARTESIAN_POINT ( 'NONE',  ( 38.26194895904384907, -22.60384086642191548, 73.11602215082116629 ) ) ;
#11267 = CARTESIAN_POINT ( 'NONE',  ( 36.80507328770344344, -5.854702703878681191, 82.78423285844689872 ) ) ;
#11268 = MECHANICAL_DESIGN_GEOMETRIC_PRESENTATION_REPRESENTATION (  '', ( #22363 ), #25222 ) ;
#11269 = B_SPLINE_CURVE_WITH_KNOTS ( 'NONE', 3,
 ( #25031, #5483, #7289, #5358 ),
 .UNSPECIFIED., .F., .F.,
 ( 4, 4 ),
 ( 0.000000000000000000, 1.000000000000000000 ),
 .UNSPECIFIED. ) ;
#11270 = B_SPLINE_CURVE_WITH_KNOTS ( 'NONE', 3,
 ( #14909, #18527, #12498, #8617 ),
 .UNSPECIFIED., .F., .F.,
 ( 4, 4 ),
 ( 0.000000000000000000, 1.000000000000000000 ),
 .UNSPECIFIED. ) ;
#11271 = CARTESIAN_POINT ( 'NONE',  ( 39.38009889167650357, -16.21368208888610596, 72.75271321436731853 ) ) ;
#11272 = ORIENTED_EDGE ( 'NONE', *, *, #22025, .T. ) ;
#11273 = CARTESIAN_POINT ( 'NONE',  ( 40.52078840805428683, -28.61368208888610454, 70.60699637195608602 ) ) ;
#11274 = VERTEX_POINT ( 'NONE', #18528 ) ;
#11275 = DIRECTION ( 'NONE',  ( 1.000000000000000000, 0.000000000000000000, 0.000000000000000000 ) ) ;
#11276 = AXIS2_PLACEMENT_3D ( 'NONE', #14950, #9419, #13153 ) ;
#11277 = DIRECTION ( 'NONE',  ( 0.000000000000000000, -0.7516416929448823669, -0.6595716529892345914 ) ) ;
#11278 = CARTESIAN_POINT ( 'NONE',  ( 39.31564783533279694, -25.30384086642191477, 70.72433947564850598 ) ) ;
#11279 = ORIENTED_EDGE ( 'NONE', *, *, #16641, .T. ) ;
#11280 = EDGE_LOOP ( 'NONE', ( #11783, #24766, #4260, #183 ) ) ;
#11281 = DIRECTION ( 'NONE',  ( -9.925461516413219746E-16, 0.8967398287344630070, 0.4425581086832393041 ) ) ;
#11282 = CIRCLE ( 'NONE', #14955, 1.000000000000000888 ) ;
#11283 = CARTESIAN_POINT ( 'NONE',  ( 43.81606138205700063, 3.913817537272060054, 6.295724427891637554 ) ) ;
#11284 = ORIENTED_EDGE ( 'NONE', *, *, #20832, .F. ) ;
#11285 = CARTESIAN_POINT ( 'NONE',  ( 43.31606138205700773, -19.34822312381089660, 24.15308711316412627 ) ) ;
#11286 = CARTESIAN_POINT ( 'NONE',  ( 38.26194895904384907, -4.603840866421914590, 73.11602215082118050 ) ) ;
#11287 = DIRECTION ( 'NONE',  ( 1.000000000000000000, 0.000000000000000000, 0.000000000000000000 ) ) ;
#11288 = CIRCLE ( 'NONE', #12520, 1.500000000000001332 ) ;
#11289 = CARTESIAN_POINT ( 'NONE',  ( 43.06606138205700063, 43.19123852234601202, 79.18605660143489899 ) ) ;
#11290 = ORIENTED_EDGE ( 'NONE', *, *, #13650, .F. ) ;
#11291 = VERTEX_POINT ( 'NONE', #20588 ) ;
#11292 = DIRECTION ( 'NONE',  ( 0.000000000000000000, 1.000000000000000000, 0.000000000000000000 ) ) ;
#11293 = COLOUR_RGB ( '', 0.72549020, 0.75294118, 0.79215686) ;
#11294 = CARTESIAN_POINT ( 'NONE',  ( 39.29254315202756231, -0.8136820888860994971, 69.94417936956673998 ) ) ;
#11295 = EDGE_CURVE ( 'NONE', #20256, #4126, #20847, .T. ) ;
#11296 = CARTESIAN_POINT ( 'NONE',  ( 38.82593461698264292, -24.70384086642191335, 73.13360434286902034 ) ) ;
#11297 = AXIS2_PLACEMENT_3D ( 'NONE', #18239, #24128, #12066 ) ;
#11298 = PRESENTATION_STYLE_ASSIGNMENT (( #7798 ) ) ;
#11299 = CARTESIAN_POINT ( 'NONE',  ( 33.31606138205700773, 7.282926244446933595, 65.60596383066929604 ) ) ;
#11300 = VERTEX_POINT ( 'NONE', #19043 ) ;
#11301 = DIRECTION ( 'NONE',  ( -1.734723475976804876E-16, -3.491481338843135327E-15, -1.000000000000000000 ) ) ;
#11302 = AXIS2_PLACEMENT_3D ( 'NONE', #5096, #11287, #20679 ) ;
#11303 = CARTESIAN_POINT ( 'NONE',  ( 43.81606138205700063, -33.39268706791821018, 60.15578316240965506 ) ) ;
#11304 = ORIENTED_EDGE ( 'NONE', *, *, #12266, .F. ) ;
#11305 = CARTESIAN_POINT ( 'NONE',  ( 28.81606138205697576, -29.47337283097074589, 44.07055847651732705 ) ) ;
#11306 = ORIENTED_EDGE ( 'NONE', *, *, #11772, .T. ) ;
#11307 = EDGE_LOOP ( 'NONE', ( #14805, #3905, #13914, #948, #4916, #23568, #24044, #6519, #4586, #8298, #3207, #4983 ) ) ;
#11308 = DIRECTION ( 'NONE',  ( -2.792262043613788535E-15, 0.8967398287344627850, 0.4425581086832399147 ) ) ;
#11309 = LINE ( 'NONE', #24536, #7826 ) ;
#11310 = EDGE_CURVE ( 'NONE', #5870, #12694, #5139, .T. ) ;
#11311 = EDGE_CURVE ( 'NONE', #23735, #1877, #20977, .T. ) ;
#11312 = CARTESIAN_POINT ( 'NONE',  ( 38.37017380507020192, -10.01368208888610312, 72.51602215082118619 ) ) ;
#11313 = ORIENTED_EDGE ( 'NONE', *, *, #2038, .T. ) ;
#11314 = VERTEX_POINT ( 'NONE', #22517 ) ;
#11315 = CARTESIAN_POINT ( 'NONE',  ( 43.06606138205700063, -38.55876147765400219, 74.30501292737012875 ) ) ;
#11316 = CARTESIAN_POINT ( 'NONE',  ( 46.81606138205701484, -19.68901644060769485, 25.93955620509757409 ) ) ;
#11317 = CARTESIAN_POINT ( 'NONE',  ( 38.93415946300896024, -23.50384086642189985, 69.66206559358661821 ) ) ;
#11318 = EDGE_CURVE ( 'NONE', #17659, #15674, #21904, .T. ) ;
#11319 = ADVANCED_FACE ( 'NONE', ( #7195 ), #9139, .F. ) ;
#11320 = ADVANCED_FACE ( 'NONE', ( #12621 ), #9269, .F. ) ;
#11321 = DIRECTION ( 'NONE',  ( 0.000000000000000000, 0.000000000000000000, 1.000000000000000000 ) ) ;
#11322 = VERTEX_POINT ( 'NONE', #16985 ) ;
#11323 = DIRECTION ( 'NONE',  ( 0.000000000000000000, 1.000000000000000000, -2.999999999999999839E-15 ) ) ;
#11324 = ADVANCED_FACE ( 'NONE', ( #24931 ), #4999, .T. ) ;
#11325 = CARTESIAN_POINT ( 'NONE',  ( 33.31606138205700773, -22.22127907754186893, 75.80501292736997243 ) ) ;
#11326 = EDGE_CURVE ( 'NONE', #7039, #3863, #12865, .T. ) ;
#11327 = CARTESIAN_POINT ( 'NONE',  ( 35.52536905565747105, -37.40916500673439771, 83.30501292737011454 ) ) ;
#11328 = CARTESIAN_POINT ( 'NONE',  ( 35.64099152588522657, 1.142818861812999742, 83.30501292736997243 ) ) ;
#11329 = DIRECTION ( 'NONE',  ( -1.849283715844614702E-16, 0.8212051873014210024, 0.5706330172266920187 ) ) ;
#11330 = AXIS2_PLACEMENT_3D ( 'NONE', #19591, #23581, #3 ) ;
#11331 = CARTESIAN_POINT ( 'NONE',  ( 43.81606138205700063, -35.41471100349711065, 71.53682070832086026 ) ) ;
#11332 = EDGE_LOOP ( 'NONE', ( #16466, #16033, #22361, #325 ) ) ;
#11333 = CARTESIAN_POINT ( 'NONE',  ( 31.81606138205700418, 18.19123852234599070, 72.05501292736995822 ) ) ;
#11334 = CARTESIAN_POINT ( 'NONE',  ( 32.31606138205700063, 9.733755362416909307, 68.18201966341686671 ) ) ;
#11335 = ORIENTED_EDGE ( 'NONE', *, *, #3112, .T. ) ;
#11336 = ORIENTED_EDGE ( 'NONE', *, *, #10193, .F. ) ;
#11337 = CARTESIAN_POINT ( 'NONE',  ( 38.37017380507018771, -9.603840866421911926, 69.04448340153881247 ) ) ;
#11338 = CARTESIAN_POINT ( 'NONE',  ( 44.81606138205700063, 40.39281886181299797, 82.55501292736983032 ) ) ;
#11339 = CARTESIAN_POINT ( 'NONE',  ( 39.29254315202756231, -14.81368208888610205, 69.94417936956672577 ) ) ;
#11340 =( NAMED_UNIT ( * ) SI_UNIT ( $, .STERADIAN. ) SOLID_ANGLE_UNIT ( ) );
#11341 = ORIENTED_EDGE ( 'NONE', *, *, #284, .F. ) ;
#11342 = CARTESIAN_POINT ( 'NONE',  ( 40.64099152588522657, -1.357181138186998925, 78.30501292736998664 ) ) ;
#11343 = CARTESIAN_POINT ( 'NONE',  ( 43.06606138205700063, 41.44123852234599070, 73.55501292736987295 ) ) ;
#11344 = CARTESIAN_POINT ( 'NONE',  ( 40.52078840805428683, -22.61368208888610454, 70.60699637195608602 ) ) ;
#11345 = AXIS2_PLACEMENT_3D ( 'NONE', #1405, #22794, #20611 ) ;
#11346 = EDGE_LOOP ( 'NONE', ( #1815, #12358, #9014, #8503 ) ) ;
#11347 = LINE ( 'NONE', #19431, #9005 ) ;
#11348 = DIRECTION ( 'NONE',  ( -1.000000000000000000, -2.999999999999999839E-15, 0.000000000000000000 ) ) ;
#11349 = FACE_OUTER_BOUND ( 'NONE', #15379, .T. ) ;
#11350 = DIRECTION ( 'NONE',  ( -1.000000000000000000, 0.000000000000000000, 0.000000000000000000 ) ) ;
#11351 = FACE_OUTER_BOUND ( 'NONE', #11483, .T. ) ;
#11352 = CARTESIAN_POINT ( 'NONE',  ( 38.37017380507018771, -11.60384086642191015, 70.24448340153877268 ) ) ;
#11353 = CARTESIAN_POINT ( 'NONE',  ( 37.25202387243752611, -1.213682088886100630, 70.00779233799264034 ) ) ;
#11354 = ORIENTED_EDGE ( 'NONE', *, *, #24838, .F. ) ;
#11355 = LINE ( 'NONE', #17270, #18499 ) ;
#11356 = EDGE_CURVE ( 'NONE', #23473, #1205, #12997, .T. ) ;
#11357 = LINE ( 'NONE', #12570, #25075 ) ;
#11358 = ORIENTED_EDGE ( 'NONE', *, *, #22759, .T. ) ;
#11359 = ORIENTED_EDGE ( 'NONE', *, *, #5167, .F. ) ;
#11360 = CARTESIAN_POINT ( 'NONE',  ( 40.14115730948191185, -1.103840866421911260, 71.43714994484034264 ) ) ;
#11361 = CARTESIAN_POINT ( 'NONE',  ( 37.69796330110504101, -1.113682088886101207, 69.66206559358663242 ) ) ;
#11362 = PRODUCT ( 'Plastic Handle Top', 'Plastic Handle Top', '', ( #11380 ) ) ;
#11363 = CARTESIAN_POINT ( 'NONE',  ( 36.07789103942398867, -5.413682088886107024, 70.70992431699450265 ) ) ;
#11364 = ORIENTED_EDGE ( 'NONE', *, *, #13056, .T. ) ;
#11365 = FACE_BOUND ( 'NONE', #8718, .T. ) ;
#11366 = CARTESIAN_POINT ( 'NONE',  ( 37.21915885897815457, -6.203840866421912459, 71.67976084211552745 ) ) ;
#11367 = LINE ( 'NONE', #7881, #8552 ) ;
#11368 = VERTEX_POINT ( 'NONE', #16718 ) ;
#11369 = DIRECTION ( 'NONE',  ( -1.000000000000000000, 1.115179377413661005E-30, 3.717264591378870232E-16 ) ) ;
#11370 = DIRECTION ( 'NONE',  ( 0.000000000000000000, -1.000000000000000000, 3.469446951953617344E-15 ) ) ;
#11371 = CARTESIAN_POINT ( 'NONE',  ( 39.02088643472237806, -10.70384086642192045, 73.73360434286902887 ) ) ;
#11372 = CARTESIAN_POINT ( 'NONE',  ( 36.51558096900348005, -21.15780082040966903, 75.86401592669550098 ) ) ;
#11373 = CARTESIAN_POINT ( 'NONE',  ( 36.31606138205700773, -21.38339321089542722, 27.67811916372966863 ) ) ;
#11374 = CARTESIAN_POINT ( 'NONE',  ( 38.82593461698262871, -14.91368208888609637, 69.62690120949091011 ) ) ;
#11375 = CARTESIAN_POINT ( 'NONE',  ( 33.80700582398852561, 3.227014992217426492, 6.369498915812663142 ) ) ;
#11376 = CARTESIAN_POINT ( 'NONE',  ( 46.98763425731077348, 1.773964314019564448, -3.427682652428131416 ) ) ;
#11377 = ORIENTED_EDGE ( 'NONE', *, *, #20927, .T. ) ;
#11378 = LINE ( 'NONE', #1560, #22917 ) ;
#11379 = CARTESIAN_POINT ( 'NONE',  ( 37.80618814713138676, -5.703840866421908018, 69.62690120949091011 ) ) ;
#11380 = PRODUCT_CONTEXT ( 'NONE', #21976, 'mechanical' ) ;
#11381 = EDGE_CURVE ( 'NONE', #2625, #21683, #14788, .T. ) ;
#11382 = DIRECTION ( 'NONE',  ( 3.614007241618344826E-17, -1.000000000000000000, 2.999999999999999839E-15 ) ) ;
#11383 = CARTESIAN_POINT ( 'NONE',  ( 38.37017380507020192, -16.01368208888610667, 73.11602215082116629 ) ) ;
#11384 = EDGE_CURVE ( 'NONE', #5709, #4360, #17113, .T. ) ;
#11385 = CARTESIAN_POINT ( 'NONE',  ( 15.14989484155900001, 36.04731275961434989, 84.30501292736985874 ) ) ;
#11386 = EDGE_CURVE ( 'NONE', #12298, #9987, #6808, .T. ) ;
#11387 = CARTESIAN_POINT ( 'NONE',  ( 37.33957961208645315, -15.80384086642190589, 69.94417936956672577 ) ) ;
#11388 = CARTESIAN_POINT ( 'NONE',  ( 36.31606138205700063, -6.943143338275722165, 83.16857229470855373 ) ) ;
#11389 = CARTESIAN_POINT ( 'NONE',  ( 36.68196826583682935, -19.61368208888610809, 71.96809898377888715 ) ) ;
#11390 = EDGE_LOOP ( 'NONE', ( #13236, #13431, #3939, #21592 ) ) ;
#11391 = CARTESIAN_POINT ( 'NONE',  ( 36.36258059203031934, -27.71368208888610596, 72.86986841596734621 ) ) ;
#11392 = ORIENTED_EDGE ( 'NONE', *, *, #5603, .F. ) ;
#11393 = DIRECTION ( 'NONE',  ( -1.000000000000000000, -1.185941393278724777E-16, -8.240782279085522416E-17 ) ) ;
#11394 = CARTESIAN_POINT ( 'NONE',  ( 43.31606138205700773, -19.28757846107943763, 24.56123906878952567 ) ) ;
#11395 = CARTESIAN_POINT ( 'NONE',  ( 37.12184278917507640, -22.10384086642191193, 71.32335560751961623 ) ) ;
#11396 = ORIENTED_EDGE ( 'NONE', *, *, #20647, .T. ) ;
#11397 = ORIENTED_EDGE ( 'NONE', *, *, #6421, .F. ) ;
#11398 = FACE_OUTER_BOUND ( 'NONE', #23903, .T. ) ;
#11399 = ADVANCED_FACE ( 'NONE', ( #7317 ), #16589, .F. ) ;
#11400 = DIRECTION ( 'NONE',  ( -1.734723475976814737E-16, -3.009265538105065873E-32, -1.000000000000000000 ) ) ;
#11401 = EDGE_LOOP ( 'NONE', ( #21066, #15563, #7107, #11565, #15552, #8118 ) ) ;
#11402 = FACE_BOUND ( 'NONE', #17929, .T. ) ;
#11403 = CARTESIAN_POINT ( 'NONE',  ( 36.89935272106205133, -26.40384086642191974, 73.23812341099225875 ) ) ;
#11404 = DIRECTION ( 'NONE',  ( -1.000000000000000000, 0.000000000000000000, 0.000000000000000000 ) ) ;
#11405 = CARTESIAN_POINT ( 'NONE',  ( 33.31606138205700773, 10.29926546647973851, 68.67466387804121553 ) ) ;
#11406 = AXIS2_PLACEMENT_3D ( 'NONE', #1283, #22419, #12898 ) ;
#11407 = ORIENTED_EDGE ( 'NONE', *, *, #25429, .T. ) ;
#11408 = AXIS2_PLACEMENT_3D ( 'NONE', #3787, #11671, #19512 ) ;
#11409 = AXIS2_PLACEMENT_3D ( 'NONE', #15748, #23603, #16630 ) ;
#11410 = CARTESIAN_POINT ( 'NONE',  ( 34.81606138205700773, -8.868983839943650693, 54.29715396818559725 ) ) ;
#11411 = CARTESIAN_POINT ( 'NONE',  ( 40.64099152588522657, 0.3928188618129990761, 80.05501292737000085 ) ) ;
#11412 = CARTESIAN_POINT ( 'NONE',  ( 39.95015449827720744, -25.00384086642191406, 71.96809898377885872 ) ) ;
#11413 =( LENGTH_UNIT ( ) NAMED_UNIT ( * ) SI_UNIT ( .MILLI., .METRE. ) );
#11414 = DIRECTION ( 'NONE',  ( 1.327674326049721180E-15, -0.4425581086832404143, 0.8967398287344625629 ) ) ;
#11415 = ORIENTED_EDGE ( 'NONE', *, *, #10595, .T. ) ;
#11416 = LINE ( 'NONE', #3290, #750 ) ;
#11417 = DIRECTION ( 'NONE',  ( -2.048868001712899108E-15, 0.6595716529892353686, -0.7516416929448815898 ) ) ;
#11418 = DIRECTION ( 'NONE',  ( -1.327674326049719602E-15, 0.4425581086832399147, -0.8967398287344627850 ) ) ;
#11419 = CARTESIAN_POINT ( 'NONE',  ( 37.89291511884479036, -4.503840866421912281, 72.49843995877331793 ) ) ;
#11420 = ORIENTED_EDGE ( 'NONE', *, *, #4114, .F. ) ;
#11421 = FACE_OUTER_BOUND ( 'NONE', #14822, .T. ) ;
#11422 = ORIENTED_EDGE ( 'NONE', *, *, #2920, .T. ) ;
#11423 = ORIENTED_EDGE ( 'NONE', *, *, #10919, .T. ) ;
#11424 = CLOSED_SHELL ( 'NONE', ( #4986, #22630, #13704, #11155, #24727, #9552, #18224, #15165, #15608, #17115, #17498, #425, #23172, #19469, #17813, #14745, #16321, #17628, #22832, #2078, #11101, #11055, #21857, #2614, #13633, #2480, #19481, #24415, #104, #17772, #3922, #20278, #12739, #10757, #5573, #5966, #12318, #1669, #9598, #12264, #13606, #21360, #10421, #1132 ) ) ;
#11425 = DIRECTION ( 'NONE',  ( -1.849283715844614702E-16, 0.8212051873014210024, 0.5706330172266920187 ) ) ;
#11426 = CARTESIAN_POINT ( 'NONE',  ( 37.21915885897815457, -13.41368208888610170, 71.08074471024443142 ) ) ;
#11427 = AXIS2_PLACEMENT_3D ( 'NONE', #19350, #9451, #19472 ) ;
#11428 = VECTOR ( 'NONE', #737, 1000.000000000000000 ) ;
#11429 = CARTESIAN_POINT ( 'NONE',  ( 39.51027997493896748, -12.51368208888610134, 71.32335560751960202 ) ) ;
#11430 = VERTEX_POINT ( 'NONE', #14655 ) ;
#11431 = ORIENTED_EDGE ( 'NONE', *, *, #22943, .T. ) ;
#11432 = ADVANCED_FACE ( 'NONE', ( #24688 ), #7062, .F. ) ;
#11433 = DIRECTION ( 'NONE',  ( -1.000000000000000000, -2.976348234363322057E-15, -2.784991061251119320E-16 ) ) ;
#11434 = ORIENTED_EDGE ( 'NONE', *, *, #1072, .T. ) ;
#11435 = CYLINDRICAL_SURFACE ( 'NONE', #16085, 1.750000000000000222 ) ;
#11436 = CARTESIAN_POINT ( 'NONE',  ( 38.82593461698265003, -14.70384086642191512, 73.13360434286903455 ) ) ;
#11437 = LINE ( 'NONE', #23517, #21483 ) ;
#11438 = CARTESIAN_POINT ( 'NONE',  ( 39.51027997493896748, -18.51368208888610312, 71.32335560751960202 ) ) ;
#11439 = ORIENTED_EDGE ( 'NONE', *, *, #19314, .T. ) ;
#11440 = EDGE_LOOP ( 'NONE', ( #12790, #8482, #17514, #22656 ) ) ;
#11441 = CARTESIAN_POINT ( 'NONE',  ( 39.32110845963273960, -5.470022085696077063, 83.30190618885059450 ) ) ;
#11442 = CARTESIAN_POINT ( 'NONE',  ( 36.31606138205700773, -21.83924545618511104, 28.60179643084731893 ) ) ;
#11443 = VECTOR ( 'NONE', #24449, 1000.000000000000000 ) ;
#11444 = B_SPLINE_CURVE_WITH_KNOTS ( 'NONE', 3,
 ( #14786, #24302, #2917, #11053, #9137, #22644, #4997, #22892, #20974, #20718, #3055, #11441, #25321, #21609, #3955, #19284, #25057, #7699 ),
 .UNSPECIFIED., .F., .F.,
 ( 4, 2, 2, 2, 2, 2, 2, 2, 4 ),
 ( 0.000000000000000000, 0.1249999999999999445, 0.2499999999999998890, 0.3749999999999998335, 0.4999999999999991673, 0.6249999999999997780, 0.7500000000000003331, 0.8749999999999994449, 1.000000000000000000 ),
 .UNSPECIFIED. ) ;
#11445 = DIRECTION ( 'NONE',  ( 0.000000000000000000, 0.4425581086832400812, -0.8967398287344626739 ) ) ;
#11446 = EDGE_CURVE ( 'NONE', #24313, #14570, #17797, .T. ) ;
#11447 = CIRCLE ( 'NONE', #14716, 3.000000000000000000 ) ;
#11448 = VECTOR ( 'NONE', #24150, 1000.000000000000000 ) ;
#11449 = ADVANCED_FACE ( 'NONE', ( #11708 ), #9897, .F. ) ;
#11450 = CARTESIAN_POINT ( 'NONE',  ( 38.44711690269065940, -5.204193249396280585, 82.80501292736992980 ) ) ;
#11451 = CYLINDRICAL_SURFACE ( 'NONE', #1136, 2.500000000000002220 ) ;
#11452 = DIRECTION ( 'NONE',  ( 1.000000000000000000, 0.000000000000000000, 0.000000000000000000 ) ) ;
#11453 = EDGE_CURVE ( 'NONE', #17862, #3296, #7615, .T. ) ;
#11454 = VERTEX_POINT ( 'NONE', #19547 ) ;
#11455 = CARTESIAN_POINT ( 'NONE',  ( 38.31606138205687984, 43.19123852234599781, 75.30501292736987295 ) ) ;
#11456 = DIRECTION ( 'NONE',  ( 8.967398287344632705E-16, -0.8967398287344631180, -0.4425581086832391375 ) ) ;
#11457 = VERTEX_POINT ( 'NONE', #21612 ) ;
#11458 = VERTEX_POINT ( 'NONE', #9387 ) ;
#11459 = CARTESIAN_POINT ( 'NONE',  ( 40.26954217208372455, -8.903840866421921518, 72.86986841596736042 ) ) ;
#11460 = EDGE_CURVE ( 'NONE', #18144, #12687, #12460, .T. ) ;
#11461 = DIRECTION ( 'NONE',  ( 1.000000000000000000, 3.083952846180990083E-15, -9.251858538542970050E-30 ) ) ;
#11462 = CARTESIAN_POINT ( 'NONE',  ( 38.26194895904383486, -15.01368208888610134, 69.64448340153877837 ) ) ;
#11463 = CIRCLE ( 'NONE', #4062, 0.5000000000000004441 ) ;
#11464 = SURFACE_SIDE_STYLE ('',( #19424 ) ) ;
#11465 = ORIENTED_EDGE ( 'NONE', *, *, #15511, .T. ) ;
#11466 = DIRECTION ( 'NONE',  ( -1.734723475976804876E-16, -3.469446951953620105E-15, -1.000000000000000000 ) ) ;
#11467 = CARTESIAN_POINT ( 'NONE',  ( 31.81606138205700418, 38.19123852234599070, 73.05501292736988717 ) ) ;
#11468 = CARTESIAN_POINT ( 'NONE',  ( 39.73277004305198545, -24.21368208888610951, 73.23812341099225875 ) ) ;
#11469 = EDGE_LOOP ( 'NONE', ( #22198, #18960, #10727, #7737 ) ) ;
#11470 = CARTESIAN_POINT ( 'NONE',  ( 31.81606138205700418, -34.67340937580780036, 71.26505871168839690 ) ) ;
#11471 = CARTESIAN_POINT ( 'NONE',  ( 33.31606138205700773, -22.22127907754187959, 75.30501292736998664 ) ) ;
#11472 = DIRECTION ( 'NONE',  ( 0.000000000000000000, -3.469446951953613400E-15, -1.000000000000000000 ) ) ;
#11473 = EDGE_CURVE ( 'NONE', #17369, #23160, #5874, .T. ) ;
#11474 = EDGE_CURVE ( 'NONE', #7685, #18044, #5764, .T. ) ;
#11475 = CARTESIAN_POINT ( 'NONE',  ( 33.31606138205700773, -11.65742039644129591, 17.30652615485722023 ) ) ;
#11476 = ADVANCED_FACE ( 'NONE', ( #3694 ), #17361, .F. ) ;
#11477 = CARTESIAN_POINT ( 'NONE',  ( 43.81606138205700063, -38.55876147765401640, 71.30501292737012875 ) ) ;
#11478 = EDGE_CURVE ( 'NONE', #9433, #2339, #7583, .T. ) ;
#11479 = CARTESIAN_POINT ( 'NONE',  ( 39.24876120206129571, -14.90384086642191264, 72.12822762946747446 ) ) ;
#11480 = CARTESIAN_POINT ( 'NONE',  ( 39.75915168707250302, -0.7136820888860997414, 70.26145752964252722 ) ) ;
#11481 = EDGE_CURVE ( 'NONE', #17202, #1848, #17500, .T. ) ;
#11482 = CIRCLE ( 'NONE', #21766, 3.000000000000002220 ) ;
#11483 = EDGE_LOOP ( 'NONE', ( #7264, #24776, #6518, #11621 ) ) ;
#11484 = DIRECTION ( 'NONE',  ( -2.412663730047099099E-15, 0.8967398287344627850, 0.4425581086832399147 ) ) ;
#11485 = LINE ( 'NONE', #13409, #23037 ) ;
#11486 = ORIENTED_EDGE ( 'NONE', *, *, #20745, .F. ) ;
#11487 = ORIENTED_EDGE ( 'NONE', *, *, #18094, .T. ) ;
#11488 = CARTESIAN_POINT ( 'NONE',  ( 38.93415946300896024, 0.4961591335780925482, 69.66206559358664663 ) ) ;
#11489 = AXIS2_PLACEMENT_3D ( 'NONE', #1414, #11600, #13526 ) ;
#11490 = CARTESIAN_POINT ( 'NONE',  ( 39.41296390513587511, -28.41368208888610525, 71.67976084211548482 ) ) ;
#11491 = CARTESIAN_POINT ( 'NONE',  ( 36.98690846071097837, -5.813682088886107380, 73.30173637941818754 ) ) ;
#11492 = VERTEX_POINT ( 'NONE', #13252 ) ;
#11493 = CARTESIAN_POINT ( 'NONE',  ( 28.84183937708599998, -34.55876147765400219, 70.30501292737000085 ) ) ;
#11494 = CARTESIAN_POINT ( 'NONE',  ( 37.89291511884479036, -2.503840866421910505, 72.49843995877331793 ) ) ;
#11495 = AXIS2_PLACEMENT_3D ( 'NONE', #9523, #3831, #19290 ) ;
#11496 = DIRECTION ( 'NONE',  ( 0.000000000000000000, 0.5706330172266919076, -0.8212051873014208914 ) ) ;
#11497 = ORIENTED_EDGE ( 'NONE', *, *, #7716, .F. ) ;
#11498 = LINE ( 'NONE', #17545, #12982 ) ;
#11499 = DIRECTION ( 'NONE',  ( -3.854941057726235139E-16, -2.999999999999999839E-15, -1.000000000000000000 ) ) ;
#11500 = CARTESIAN_POINT ( 'NONE',  ( 40.26954217208372455, -8.903840866421921518, 72.86986841596736042 ) ) ;
#11501 = LINE ( 'NONE', #7756, #24749 ) ;
#11502 = AXIS2_PLACEMENT_3D ( 'NONE', #21256, #23180, #3352 ) ;
#11503 = CARTESIAN_POINT ( 'NONE',  ( 37.69796330110504101, -17.11368208888610098, 69.66206559358661821 ) ) ;
#11504 = CARTESIAN_POINT ( 'NONE',  ( 33.77225884907574027, 2.787429531901909119, 6.090838246671958167 ) ) ;
#11505 = EDGE_CURVE ( 'NONE', #21683, #18450, #25190, .T. ) ;
#11506 = DIRECTION ( 'NONE',  ( 0.000000000000000000, 1.000000000000000000, -3.469446951953613400E-15 ) ) ;
#11507 = VECTOR ( 'NONE', #16210, 1000.000000000000227 ) ;
#11508 = VERTEX_POINT ( 'NONE', #11327 ) ;
#11509 = LINE ( 'NONE', #17553, #3590 ) ;
#11510 = CARTESIAN_POINT ( 'NONE',  ( 39.29254315202757653, -10.80384086642191477, 72.81632618279323310 ) ) ;
#11511 = APPLICATION_PROTOCOL_DEFINITION ( 'draft international standard', 'automotive_design', 1998, #5680 ) ;
#11512 = DIRECTION ( 'NONE',  ( -1.510383499235849534E-16, -0.1218693434051499741, -0.9925461516413217611 ) ) ;
#11513 = VECTOR ( 'NONE', #18140, 1000.000000000000000 ) ;
#11514 = CARTESIAN_POINT ( 'NONE',  ( 36.68196826583682935, -19.61368208888610809, 71.96809898377888715 ) ) ;
#11515 = VECTOR ( 'NONE', #8877, 1000.000000000000000 ) ;
#11516 = CARTESIAN_POINT ( 'NONE',  ( 33.31606138205700773, 3.296535697557910538, 65.33616386252352015 ) ) ;
#11517 = CARTESIAN_POINT ( 'NONE',  ( 38.93415946300896024, -19.50384086642191050, 69.66206559358661821 ) ) ;
#11518 = CARTESIAN_POINT ( 'NONE',  ( 36.31606138205700063, -6.859540048202029894, 82.67032472249573516 ) ) ;
#11519 = VECTOR ( 'NONE', #6940, 1000.000000000000000 ) ;
#11520 = CARTESIAN_POINT ( 'NONE',  ( 38.26194895904383486, -21.01368208888610312, 69.64448340153877837 ) ) ;
#11521 = EDGE_LOOP ( 'NONE', ( #25311, #8567, #24237, #13159 ) ) ;
#11522 = CARTESIAN_POINT ( 'NONE',  ( 36.29569395875879678, -25.31368208888610027, 69.98269868914866265 ) ) ;
#11523 = ORIENTED_EDGE ( 'NONE', *, *, #2777, .T. ) ;
#11524 = DIRECTION ( 'NONE',  ( 4.336808689942074435E-17, -1.000000000000000000, 3.491481338843135327E-15 ) ) ;
#11525 = DIRECTION ( 'NONE',  ( 0.000000000000000000, -3.469446951953611033E-15, 1.000000000000000000 ) ) ;
#11526 = CARTESIAN_POINT ( 'NONE',  ( 38.73920764526923932, -27.50384086642191406, 70.26206559358661252 ) ) ;
#11527 = AXIS2_PLACEMENT_3D ( 'NONE', #22882, #19151, #1487 ) ;
#11528 = EDGE_LOOP ( 'NONE', ( #1695, #5975, #23522, #24804 ) ) ;
#11529 = ORIENTED_EDGE ( 'NONE', *, *, #9180, .F. ) ;
#11530 = DIRECTION ( 'NONE',  ( -1.933202721249430383E-16, 0.9925461516413217611, -0.1218693434051499741 ) ) ;
#11531 = PLANE ( 'NONE',  #7539 ) ;
#11532 = ORIENTED_EDGE ( 'NONE', *, *, #9133, .T. ) ;
#11533 = CARTESIAN_POINT ( 'NONE',  ( 43.31606138205700063, -10.19550266980812658, 14.63954348514304904 ) ) ;
#11534 = CARTESIAN_POINT ( 'NONE',  ( 38.37017380507018771, -29.60384086642191193, 69.04448340153878405 ) ) ;
#11535 = ADVANCED_FACE ( 'NONE', ( #7831 ), #15426, .F. ) ;
#11536 = EDGE_CURVE ( 'NONE', #22091, #21703, #21501, .T. ) ;
#11537 = LINE ( 'NONE', #5851, #10482 ) ;
#11538 = DIRECTION ( 'NONE',  ( 0.000000000000000000, 0.6568589528324746407, -0.7540134720837716742 ) ) ;
#11539 = EDGE_LOOP ( 'NONE', ( #6743, #16066, #5291, #9732 ) ) ;
#11540 = CARTESIAN_POINT ( 'NONE',  ( 33.97785981915764353, 3.164009542016340770, 6.379277577726464088 ) ) ;
#11541 = DIRECTION ( 'NONE',  ( 1.000000000000000000, 0.000000000000000000, 0.000000000000000000 ) ) ;
#11542 = ORIENTED_EDGE ( 'NONE', *, *, #4498, .T. ) ;
#11543 = CARTESIAN_POINT ( 'NONE',  ( 36.64852494920107517, -28.20384086642191335, 71.86517103874047052 ) ) ;
#11544 = FILL_AREA_STYLE ('',( #15395 ) ) ;
#11545 = DIRECTION ( 'NONE',  ( 1.000000000000000000, 0.000000000000000000, 0.000000000000000000 ) ) ;
#11546 = ORIENTED_EDGE ( 'NONE', *, *, #15413, .F. ) ;
#11547 = AXIS2_PLACEMENT_3D ( 'NONE', #5428, #21147, #19844 ) ;
#11548 = FACE_OUTER_BOUND ( 'NONE', #16402, .T. ) ;
#11549 = EDGE_CURVE ( 'NONE', #23228, #17369, #19164, .T. ) ;
#11550 = AXIS2_PLACEMENT_3D ( 'NONE', #6033, #23915, #20192 ) ;
#11551 = PLANE ( 'NONE',  #15610 ) ;
#11552 = CARTESIAN_POINT ( 'NONE',  ( 36.56606138205700063, 5.719301844480432884, 2.701924129460374413 ) ) ;
#11553 = CARTESIAN_POINT ( 'NONE',  ( 37.60469502381300799, -4.403840866421911748, 72.26730301774236409 ) ) ;
#11554 = EDGE_LOOP ( 'NONE', ( #8012, #10870, #12642, #23769 ) ) ;
#11555 = CARTESIAN_POINT ( 'NONE',  ( 44.81606138205700063, 44.92314894770293421, 80.37823623207322044 ) ) ;
#11556 = ORIENTED_EDGE ( 'NONE', *, *, #16105, .F. ) ;
#11557 = ORIENTED_EDGE ( 'NONE', *, *, #22629, .T. ) ;
#11558 = DIRECTION ( 'NONE',  ( -1.000000000000000000, 1.115179377413661005E-30, 3.717264591378870232E-16 ) ) ;
#11559 = CARTESIAN_POINT ( 'NONE',  ( 37.25260217561390874, -13.61368208888610098, 71.78268878715392987 ) ) ;
#11560 = CARTESIAN_POINT ( 'NONE',  ( 39.24876120206128860, -10.71368208888610063, 70.63227792289247020 ) ) ;
#11561 = ORIENTED_EDGE ( 'NONE', *, *, #22452, .F. ) ;
#11562 = ORIENTED_EDGE ( 'NONE', *, *, #25318, .T. ) ;
#11563 = DIRECTION ( 'NONE',  ( -1.156482317317870492E-16, -0.4425581086832399702, 0.8967398287344626739 ) ) ;
#11564 = CARTESIAN_POINT ( 'NONE',  ( 33.33121445922205339, -32.87633672316712108, 59.29685926994373091 ) ) ;
#11565 = ORIENTED_EDGE ( 'NONE', *, *, #13511, .T. ) ;
#11566 = LINE ( 'NONE', #19404, #12813 ) ;
#11567 = CARTESIAN_POINT ( 'NONE',  ( 39.75915168707251723, -16.90384086642191619, 72.49904802271738902 ) ) ;
#11568 = EDGE_CURVE ( 'NONE', #17202, #947, #3800, .T. ) ;
#11569 = EDGE_CURVE ( 'NONE', #17699, #17085, #19671, .T. ) ;
#11570 = AXIS2_PLACEMENT_3D ( 'NONE', #4075, #1869, #192 ) ;
#11571 = CARTESIAN_POINT ( 'NONE',  ( 38.31606138205700063, -22.22127907754186893, 75.55501292736998664 ) ) ;
#11572 = CARTESIAN_POINT ( 'NONE',  ( 39.24876120206128860, -20.71368208888610596, 70.63227792289245599 ) ) ;
#11573 = AXIS2_PLACEMENT_3D ( 'NONE', #18764, #1096, #8985 ) ;
#11574 = ORIENTED_EDGE ( 'NONE', *, *, #17211, .F. ) ;
#11575 = CARTESIAN_POINT ( 'NONE',  ( 43.05893253799203535, 3.408563886989315339, 6.350990360017436664 ) ) ;
#11576 = DIRECTION ( 'NONE',  ( 0.000000000000000000, 0.6568589528324745297, -0.7540134720837717852 ) ) ;
#11577 = CARTESIAN_POINT ( 'NONE',  ( 43.81606138205700063, 28.12806996228107081, 65.30501292736992980 ) ) ;
#11578 = CARTESIAN_POINT ( 'NONE',  ( 39.54057891361352972, -5.617364314676576598, 83.29713963190137349 ) ) ;
#11579 = CARTESIAN_POINT ( 'NONE',  ( 31.81606138205700418, 24.50429740018177682, 101.9912164131601457 ) ) ;
#11580 = EDGE_CURVE ( 'NONE', #947, #3835, #5385, .T. ) ;
#11581 = PRODUCT_DEFINITION_SHAPE ( 'NONE', 'NONE',  #10107 ) ;
#11582 = DIRECTION ( 'NONE',  ( -1.000000000000000000, 0.000000000000000000, 0.000000000000000000 ) ) ;
#11583 = ORIENTED_EDGE ( 'NONE', *, *, #8479, .F. ) ;
#11584 = DIRECTION ( 'NONE',  ( 1.734723475976814737E-16, 3.009265538105065873E-32, 1.000000000000000000 ) ) ;
#11585 = VERTEX_POINT ( 'NONE', #25324 ) ;
#11586 = VERTEX_POINT ( 'NONE', #7702 ) ;
#11587 = AXIS2_PLACEMENT_3D ( 'NONE', #11183, #15797, #17737 ) ;
#11588 = CARTESIAN_POINT ( 'NONE',  ( 36.29569395875881099, -12.30384086642192010, 72.77780686321128201 ) ) ;
#11589 = DIRECTION ( 'NONE',  ( -1.000000000000000000, 0.000000000000000000, 0.000000000000000000 ) ) ;
#11590 = CARTESIAN_POINT ( 'NONE',  ( 37.80618814713140097, -17.91368208888609814, 73.13360434286903455 ) ) ;
#11591 = ORIENTED_EDGE ( 'NONE', *, *, #20261, .F. ) ;
#11592 = LINE ( 'NONE', #15182, #25181 ) ;
#11593 = CARTESIAN_POINT ( 'NONE',  ( 38.31606138205700063, 40.69123852234599781, 71.30501292737000085 ) ) ;
#11594 = CARTESIAN_POINT ( 'NONE',  ( 36.29569395875879678, -23.31368208888610383, 69.98269868914866265 ) ) ;
#11595 = ORIENTED_EDGE ( 'NONE', *, *, #1881, .F. ) ;
#11596 = DIRECTION ( 'NONE',  ( 0.000000000000000000, 1.000000000000000000, -2.999999999999999839E-15 ) ) ;
#11597 = FACE_OUTER_BOUND ( 'NONE', #9861, .T. ) ;
#11598 = LINE ( 'NONE', #21249, #7933 ) ;
#11599 = SURFACE_SIDE_STYLE ('',( #23557 ) ) ;
#11600 = DIRECTION ( 'NONE',  ( -1.000000000000000000, -1.000000000000000078E-15, 0.000000000000000000 ) ) ;
#11601 = ADVANCED_FACE ( 'NONE', ( #2268 ), #12211, .F. ) ;
#11602 = CARTESIAN_POINT ( 'NONE',  ( 36.81465384343994884, 42.38065457974295924, 79.52109337493035923 ) ) ;
#11603 = CARTESIAN_POINT ( 'NONE',  ( 38.73920764526923932, -9.503840866421912281, 70.26206559358664094 ) ) ;
#11604 = CARTESIAN_POINT ( 'NONE',  ( 37.12184278917507640, -27.51368208888609956, 71.43714994484032843 ) ) ;
#11605 = VERTEX_POINT ( 'NONE', #10270 ) ;
#11606 = CARTESIAN_POINT ( 'NONE',  ( 40.31606138205700773, 8.691238522346996120, 69.09790614618343341 ) ) ;
#11607 = DIRECTION ( 'NONE',  ( 0.000000000000000000, -0.7516416929448823669, -0.6595716529892345914 ) ) ;
#11608 = EDGE_LOOP ( 'NONE', ( #6403, #12878, #13789, #10704 ) ) ;
#11609 = ORIENTED_EDGE ( 'NONE', *, *, #6906, .T. ) ;
#11610 = CARTESIAN_POINT ( 'NONE',  ( 36.87297107704149823, 0.09615913357809147133, 70.26145752964255564 ) ) ;
#11611 = CARTESIAN_POINT ( 'NONE',  ( 38.00113996487114321, -27.91368208888610170, 72.53360434286901182 ) ) ;
#11612 = CARTESIAN_POINT ( 'NONE',  ( 39.64521430340304420, -4.813682088886099386, 69.45876917294177133 ) ) ;
#11613 = VECTOR ( 'NONE', #19924, 1000.000000000000227 ) ;
#11614 = ORIENTED_EDGE ( 'NONE', *, *, #5799, .F. ) ;
#11615 = FACE_OUTER_BOUND ( 'NONE', #12788, .T. ) ;
#11616 = VECTOR ( 'NONE', #10158, 1000.000000000000227 ) ;
#11617 = CARTESIAN_POINT ( 'NONE',  ( 37.38336156205273397, -7.903840866421910860, 70.63227792289248441 ) ) ;
#11618 = EDGE_CURVE ( 'NONE', #1658, #3066, #16184, .T. ) ;
#11619 = DIRECTION ( 'NONE',  ( -1.000000000000000000, 1.927470528863119788E-16, -5.782411586589358909E-31 ) ) ;
#11620 = EDGE_CURVE ( 'NONE', #5274, #13966, #6524, .T. ) ;
#11621 = ORIENTED_EDGE ( 'NONE', *, *, #19958, .F. ) ;
#11622 = DIRECTION ( 'NONE',  ( -1.000000000000000000, 0.000000000000000000, 1.734723475976804876E-16 ) ) ;
#11623 = PLANE ( 'NONE',  #19079 ) ;
#11624 = AXIS2_PLACEMENT_3D ( 'NONE', #24290, #18273, #8734 ) ;
#11625 = CARTESIAN_POINT ( 'NONE',  ( 37.61123632939164452, -7.703840866421914235, 69.02690120949094421 ) ) ;
#11626 = ADVANCED_FACE ( 'NONE', ( #6022 ), #22109, .T. ) ;
#11627 = EDGE_CURVE ( 'NONE', #6631, #12000, #14261, .T. ) ;
#11628 = ADVANCED_FACE ( 'NONE', ( #21990, #20055, #23784, #24036 ), #4599, .T. ) ;
#11629 = DIRECTION ( 'NONE',  ( 1.000000000000000000, 3.001186103030333510E-15, 2.281710121244060993E-16 ) ) ;
#11630 = CARTESIAN_POINT ( 'NONE',  ( 36.64852494920107517, -11.41368208888610525, 70.89533451361947414 ) ) ;
#11631 = DIRECTION ( 'NONE',  ( -2.690219486203388234E-15, 0.8967398287344627850, 0.4425581086832399147 ) ) ;
#11632 = CARTESIAN_POINT ( 'NONE',  ( 38.31606138205700063, 29.91058581477919986, 95.51211970855651145 ) ) ;
#11633 = ORIENTED_EDGE ( 'NONE', *, *, #19801, .F. ) ;
#11634 = DIRECTION ( 'NONE',  ( 0.000000000000000000, 0.6568589528324747517, -0.7540134720837718962 ) ) ;
#11635 = EDGE_CURVE ( 'NONE', #13053, #10990, #14138, .T. ) ;
#11636 = CARTESIAN_POINT ( 'NONE',  ( 36.80608444377002542, -4.303840866421916544, 72.40698646996135324 ) ) ;
#11638 = EDGE_CURVE ( 'NONE', #2876, #828, #2517, .T. ) ;
#11637 = APPLICATION_PROTOCOL_DEFINITION ( 'draft international standard', 'automotive_design', 1998, #21976 ) ;
#11639 = AXIS2_PLACEMENT_3D ( 'NONE', #2919, #22771, #11057 ) ;
#11640 = CARTESIAN_POINT ( 'NONE',  ( 33.49067756756858927, 3.520309816310820406, 6.331808112780875852 ) ) ;
#11641 = CARTESIAN_POINT ( 'NONE',  ( 36.68196826583682935, -21.61368208888610454, 71.96809898377888715 ) ) ;
#11642 = CARTESIAN_POINT ( 'NONE',  ( 43.31606138205700063, -22.22127907754187959, 75.30501292736998664 ) ) ;
#11643 = VECTOR ( 'NONE', #9378, 1000.000000000000227 ) ;
#11644 = CARTESIAN_POINT ( 'NONE',  ( 38.93415946300896024, -17.50384086642190695, 69.66206559358661821 ) ) ;
#11645 = FACE_OUTER_BOUND ( 'NONE', #25201, .T. ) ;
#11646 = EDGE_CURVE ( 'NONE', #8412, #22152, #10398, .T. ) ;
#11647 = CIRCLE ( 'NONE', #12056, 0.7500000000000006661 ) ;
#11648 = CARTESIAN_POINT ( 'NONE',  ( 40.14115730948191185, -16.51368208888610667, 71.32335560751960202 ) ) ;
#11649 = EDGE_LOOP ( 'NONE', ( #9057, #23184, #238, #24077, #8956, #20542 ) ) ;
#11650 = CARTESIAN_POINT ( 'NONE',  ( 38.26194895904383486, -21.01368208888610312, 69.04448340153878405 ) ) ;
#11651 = CIRCLE ( 'NONE', #2573, 1.249999999999996891 ) ;
#11652 = EDGE_LOOP ( 'NONE', ( #14674, #21255, #1098, #15642 ) ) ;
#11653 = DIRECTION ( 'NONE',  ( 1.000000000000000000, 8.673617379884027583E-16, 0.000000000000000000 ) ) ;
#11654 = DIRECTION ( 'NONE',  ( 0.000000000000000000, -1.000000000000000000, 0.000000000000000000 ) ) ;
#11655 = CARTESIAN_POINT ( 'NONE',  ( 37.12184278917507640, -24.10384086642191193, 71.32335560751960202 ) ) ;
#11656 = ORIENTED_EDGE ( 'NONE', *, *, #10556, .F. ) ;
#11657 = ORIENTED_EDGE ( 'NONE', *, *, #12651, .T. ) ;
#11658 = LINE ( 'NONE', #17832, #6356 ) ;
#11659 = CARTESIAN_POINT ( 'NONE',  ( 40.31606138205700773, -1.357181138186124736, 83.30501292736991559 ) ) ;
#11661 = AXIS2_PLACEMENT_3D ( 'NONE', #13823, #26, #13574 ) ;
#11660 = FACE_OUTER_BOUND ( 'NONE', #20809, .T. ) ;
#11662 = CARTESIAN_POINT ( 'NONE',  ( 38.93415946300896024, 0.4961591335780925482, 69.66206559358664663 ) ) ;
#11663 = CIRCLE ( 'NONE', #4244, 3.999999999999899636 ) ;
#11664 = DIRECTION ( 'NONE',  ( 0.000000000000000000, 1.000000000000000000, -2.775557561562891351E-15 ) ) ;
#11665 = CARTESIAN_POINT ( 'NONE',  ( 40.52078840805428683, -4.613682088886104538, 70.60699637195608602 ) ) ;
#11666 = CIRCLE ( 'NONE', #10006, 3.000000000000002665 ) ;
#11667 = CARTESIAN_POINT ( 'NONE',  ( 33.31606138205700773, -16.77230293220685198, 77.52306850662458260 ) ) ;
#11668 = ORIENTED_EDGE ( 'NONE', *, *, #25139, .F. ) ;
#11669 = EDGE_LOOP ( 'NONE', ( #22852, #10743, #5714, #24761 ) ) ;
#11670 = DIRECTION ( 'NONE',  ( -3.771137991253929559E-16, 0.8212051873014208914, 0.5706330172266919076 ) ) ;
#11671 = DIRECTION ( 'NONE',  ( 0.000000000000000000, -2.999999999999999839E-15, -1.000000000000000000 ) ) ;
#11672 = CIRCLE ( 'NONE', #20280, 0.7500000000000006661 ) ;
#11673 = CARTESIAN_POINT ( 'NONE',  ( 36.80608444377002542, -22.30384086642191477, 72.40698646996133903 ) ) ;
#11674 =( NAMED_UNIT ( * ) SI_UNIT ( $, .STERADIAN. ) SOLID_ANGLE_UNIT ( ) );
#11675 = CARTESIAN_POINT ( 'NONE',  ( 42.06606138205700063, 45.04446929126260102, 82.37823623207320622 ) ) ;
#11676 = ORIENTED_EDGE ( 'NONE', *, *, #19005, .T. ) ;
#11677 = FACE_OUTER_BOUND ( 'NONE', #23537, .T. ) ;
#11678 = VECTOR ( 'NONE', #14722, 1000.000000000000000 ) ;
#11679 = CARTESIAN_POINT ( 'NONE',  ( 39.31606138205700063, 16.19123852234700678, 71.30501292736995822 ) ) ;
#11680 = CYLINDRICAL_SURFACE ( 'NONE', #24534, 4.000000000000003553 ) ;
#11681 = CARTESIAN_POINT ( 'NONE',  ( 37.60469502381300799, -6.403840866421910860, 72.26730301774236409 ) ) ;
#11682 = VERTEX_POINT ( 'NONE', #8087 ) ;
#11683 = EDGE_CURVE ( 'NONE', #21641, #5590, #208, .T. ) ;
#11684 = AXIS2_PLACEMENT_3D ( 'NONE', #7369, #25111, #3744 ) ;
#11685 = CARTESIAN_POINT ( 'NONE',  ( 34.81606138205687273, 33.19123852234595518, 61.80501292736990848 ) ) ;
#11686 = ORIENTED_EDGE ( 'NONE', *, *, #4866, .T. ) ;
#11687 = EDGE_CURVE ( 'NONE', #18550, #3395, #12087, .T. ) ;
#11688 = ORIENTED_EDGE ( 'NONE', *, *, #5219, .T. ) ;
#11689 = FACE_OUTER_BOUND ( 'NONE', #1074, .T. ) ;
#11690 = CARTESIAN_POINT ( 'NONE',  ( 37.89291511884476904, -9.113682088886102761, 70.26206559358664094 ) ) ;
#11691 = CARTESIAN_POINT ( 'NONE',  ( 38.63098279924288647, -10.91368208888610170, 70.22690120949091863 ) ) ;
#11692 = ORIENTED_EDGE ( 'NONE', *, *, #17429, .T. ) ;
#11693 = AXIS2_PLACEMENT_3D ( 'NONE', #25482, #24747, #7729 ) ;
#11694 = VERTEX_POINT ( 'NONE', #590 ) ;
#11695 = LINE ( 'NONE', #19401, #846 ) ;
#11696 = DIRECTION ( 'NONE',  ( 0.000000000000000000, -0.6568589528324746407, 0.7540134720837716742 ) ) ;
#11697 = ORIENTED_EDGE ( 'NONE', *, *, #20830, .F. ) ;
#11698 = CARTESIAN_POINT ( 'NONE',  ( 38.37017380507020192, 1.986317911113890444, 73.11602215082119471 ) ) ;
#11699 = CARTESIAN_POINT ( 'NONE',  ( 39.29254315202757653, -16.80384086642191477, 72.81632618279321889 ) ) ;
#11700 = CARTESIAN_POINT ( 'NONE',  ( 42.99533163877982389, 2.835194748544836330, 6.100154062548608813 ) ) ;
#11701 = CARTESIAN_POINT ( 'NONE',  ( 38.73920764526925353, -18.11368208888610098, 72.49843995877330372 ) ) ;
#11702 = ORIENTED_EDGE ( 'NONE', *, *, #22711, .T. ) ;
#11703 = CIRCLE ( 'NONE', #555, 1.000000000000000888 ) ;
#11704 = ORIENTED_EDGE ( 'NONE', *, *, #24021, .F. ) ;
#11705 = DIRECTION ( 'NONE',  ( -1.000000000000000000, 0.000000000000000000, 0.000000000000000000 ) ) ;
#11706 = CARTESIAN_POINT ( 'NONE',  ( 36.68196826583682935, -15.61368208888610454, 71.96809898377888715 ) ) ;
#11707 = CARTESIAN_POINT ( 'NONE',  ( 31.81606138205700418, -36.30035594811090505, 74.91924054225879104 ) ) ;
#11708 = FACE_OUTER_BOUND ( 'NONE', #22440, .T. ) ;
#11709 = DIRECTION ( 'NONE',  ( 1.000000000000000000, 0.000000000000000000, 0.000000000000000000 ) ) ;
#11710 = CARTESIAN_POINT ( 'NONE',  ( 33.31606138205700773, 7.187001342539796944, 66.09667597968754649 ) ) ;
#11711 = ADVANCED_FACE ( 'NONE', ( #16057 ), #8467, .T. ) ;
#11712 = CARTESIAN_POINT ( 'NONE',  ( 46.81606138205700063, -13.43064139120326672, 11.56373968489310755 ) ) ;
#11713 = EDGE_CURVE ( 'NONE', #235, #1130, #12887, .T. ) ;
#11714 = ORIENTED_EDGE ( 'NONE', *, *, #15060, .T. ) ;
#11715 = EDGE_CURVE ( 'NONE', #16916, #1296, #13880, .T. ) ;
#11716 = LINE ( 'NONE', #19554, #20583 ) ;
#11717 = ORIENTED_EDGE ( 'NONE', *, *, #7607, .T. ) ;
#11718 = ORIENTED_EDGE ( 'NONE', *, *, #15530, .T. ) ;
#11719 = VECTOR ( 'NONE', #407, 1000.000000000000000 ) ;
#11720 = VECTOR ( 'NONE', #74, 1000.000000000000000 ) ;
#11721 = CARTESIAN_POINT ( 'NONE',  ( 40.77203464402485622, -11.10384086642191193, 71.43714994484034264 ) ) ;
#11722 = VERTEX_POINT ( 'NONE', #18377 ) ;
#11723 = CYLINDRICAL_SURFACE ( 'NONE', #7487, 2.500000000000002220 ) ;
#11724 = CARTESIAN_POINT ( 'NONE',  ( 39.82603832034400426, -16.31368208888610738, 72.40698646996133903 ) ) ;
#11725 = SURFACE_STYLE_USAGE ( .BOTH. , #11464 ) ;
#11726 = ORIENTED_EDGE ( 'NONE', *, *, #14752, .F. ) ;
#11727 = CARTESIAN_POINT ( 'NONE',  ( 40.81606138205700773, 37.44123852234599781, 75.30501292736990138 ) ) ;
#11728 = LINE ( 'NONE', #9535, #23182 ) ;
#11729 = EDGE_CURVE ( 'NONE', #2388, #3119, #1751, .T. ) ;
#11730 = CARTESIAN_POINT ( 'NONE',  ( 38.37017380507020192, -20.01368208888611022, 73.71602215082113219 ) ) ;
#11731 = EDGE_LOOP ( 'NONE', ( #25197, #15301, #8732, #10766 ) ) ;
#11732 = CARTESIAN_POINT ( 'NONE',  ( 43.81606138205700063, 46.92314894770294131, 80.37823623207322044 ) ) ;
#11733 = CARTESIAN_POINT ( 'NONE',  ( 43.31606138205700063, -37.53049398575952722, 70.06662099985003067 ) ) ;
#11734 = CARTESIAN_POINT ( 'NONE',  ( 30.81606138205700418, -38.55876147765410167, 66.30501292737000085 ) ) ;
#11735 = EDGE_LOOP ( 'NONE', ( #12583, #25434, #16864, #1360 ) ) ;
#11736 = AXIS2_PLACEMENT_3D ( 'NONE', #11247, #2844, #1170 ) ;
#11737 = LINE ( 'NONE', #19569, #19845 ) ;
#11738 = LINE ( 'NONE', #5795, #4886 ) ;
#11739 = DIRECTION ( 'NONE',  ( -1.000000000000000000, 0.000000000000000000, 0.000000000000000000 ) ) ;
#11740 = CARTESIAN_POINT ( 'NONE',  ( 39.51027997493896748, -13.10384086642191015, 71.43714994484032843 ) ) ;
#11741 = CARTESIAN_POINT ( 'NONE',  ( 36.87297107704152666, 0.2863179111138939303, 72.49904802271743165 ) ) ;
#11742 = ORIENTED_EDGE ( 'NONE', *, *, #6714, .F. ) ;
#11743 = DIRECTION ( 'NONE',  ( 0.000000000000000000, 0.9814242980364923374, 0.1918498038142812112 ) ) ;
#11744 = CARTESIAN_POINT ( 'NONE',  ( 38.31606138205700063, 40.69123852234599781, 71.30501292737000085 ) ) ;
#11745 = VERTEX_POINT ( 'NONE', #19933 ) ;
#11746 = EDGE_LOOP ( 'NONE', ( #23543, #23975, #7456 ) ) ;
#11747 = CARTESIAN_POINT ( 'NONE',  ( 36.11133435605973574, -28.00384086642191761, 70.60699637195608602 ) ) ;
#11748 = CARTESIAN_POINT ( 'NONE',  ( 38.26194895904383486, -23.01368208888610312, 70.24448340153875847 ) ) ;
#11749 = CARTESIAN_POINT ( 'NONE',  ( 40.26954217208371034, -4.713682088886099741, 69.89063713639259845 ) ) ;
#11750 = ORIENTED_EDGE ( 'NONE', *, *, #13822, .T. ) ;
#11751 = CARTESIAN_POINT ( 'NONE',  ( 44.06606138205700063, 29.91058581477919986, 95.51211970855651145 ) ) ;
#11752 = VECTOR ( 'NONE', #11622, 1000.000000000000000 ) ;
#11753 = CARTESIAN_POINT ( 'NONE',  ( 38.93987200065210175, -2.803840866421911660, 72.33091598616827866 ) ) ;
#11754 = DIRECTION ( 'NONE',  ( 1.000000000000000000, 1.734723475976804876E-16, -1.734723475976814737E-16 ) ) ;
#11755 = ORIENTED_EDGE ( 'NONE', *, *, #14287, .F. ) ;
#11756 = DIRECTION ( 'NONE',  ( 0.000000000000000000, 1.000000000000000000, -2.999999999999999839E-15 ) ) ;
#11757 = CARTESIAN_POINT ( 'NONE',  ( 40.81606138205700773, 37.44123852234599781, 74.30501292736988717 ) ) ;
#11758 = ADVANCED_FACE ( 'NONE', ( #21735 ), #11965, .T. ) ;
#11759 = CARTESIAN_POINT ( 'NONE',  ( 36.07789103942399578, -10.20384086642191690, 72.05058123536544201 ) ) ;
#11760 = DIRECTION ( 'NONE',  ( 1.067465804653198538E-15, -0.4425581086832399147, 0.8967398287344627850 ) ) ;
#11761 = CARTESIAN_POINT ( 'NONE',  ( 43.81606138205700063, -35.82531359714782582, 71.25150419970752580 ) ) ;
#11762 = CARTESIAN_POINT ( 'NONE',  ( 37.25202387243752611, -13.21368208888610063, 70.00779233799262613 ) ) ;
#11763 = DIRECTION ( 'NONE',  ( -2.690219486203388234E-15, 0.8967398287344627850, 0.4425581086832399147 ) ) ;
#11764 = FACE_OUTER_BOUND ( 'NONE', #20740, .T. ) ;
#11765 = DIRECTION ( 'NONE',  ( -1.000000000000000000, 3.009265538105049890E-31, 1.734723475976809806E-16 ) ) ;
#11766 = CARTESIAN_POINT ( 'NONE',  ( 36.64852494920107517, -2.203840866421912015, 71.86517103874049894 ) ) ;
#11767 = FACE_OUTER_BOUND ( 'NONE', #18830, .T. ) ;
#11768 = EDGE_CURVE ( 'NONE', #17862, #6624, #10655, .T. ) ;
#11769 = CARTESIAN_POINT ( 'NONE',  ( 38.26194895904383486, -21.01368208888610312, 69.64448340153877837 ) ) ;
#11770 = EDGE_CURVE ( 'NONE', #14052, #17340, #8976, .T. ) ;
#11771 = CARTESIAN_POINT ( 'NONE',  ( 40.31606138205701484, -22.71854986786759056, 31.51329497139233737 ) ) ;
#11772 = EDGE_CURVE ( 'NONE', #10846, #5334, #9200, .T. ) ;
#11773 = CARTESIAN_POINT ( 'NONE',  ( 39.95015449827720744, -19.00384086642191406, 71.96809898377887293 ) ) ;
#11774 = ADVANCED_FACE ( 'NONE', ( #965 ), #14879, .T. ) ;
#11775 = CARTESIAN_POINT ( 'NONE',  ( 38.31606138205700063, 37.69123852234599781, 71.30501292737001506 ) ) ;
#11776 = CARTESIAN_POINT ( 'NONE',  ( 39.75915168707250302, -12.71368208888610063, 70.26145752964251301 ) ) ;
#11777 = ORIENTED_EDGE ( 'NONE', *, *, #23995, .F. ) ;
#11778 = CARTESIAN_POINT ( 'NONE',  ( 39.73277004305198545, -24.21368208888610951, 73.23812341099225875 ) ) ;
#11779 = ORIENTED_EDGE ( 'NONE', *, *, #20081, .T. ) ;
#11780 = DIRECTION ( 'NONE',  ( 1.000000000000000275E-15, -0.9439899321577401858, -0.3299742535180970604 ) ) ;
#11781 = DIRECTION ( 'NONE',  ( 1.734723475976804876E-16, 3.552713678800500140E-15, 1.000000000000000000 ) ) ;
#11782 = CARTESIAN_POINT ( 'NONE',  ( 37.89291511884479036, -26.50384086642191406, 72.49843995877328950 ) ) ;
#11783 = ORIENTED_EDGE ( 'NONE', *, *, #15398, .F. ) ;
#11784 = ORIENTED_EDGE ( 'NONE', *, *, #7674, .T. ) ;
#11785 = CARTESIAN_POINT ( 'NONE',  ( 42.68042513965293949, 2.191238522347003226, 70.30501292737000085 ) ) ;
#11786 = DIRECTION ( 'NONE',  ( -1.000000000000000000, 0.000000000000000000, -0.000000000000000000 ) ) ;
#11787 = EDGE_CURVE ( 'NONE', #5237, #16332, #24526, .T. ) ;
#11788 = LINE ( 'NONE', #10444, #9009 ) ;
#11789 = CARTESIAN_POINT ( 'NONE',  ( 39.38009889167648936, 0.5961591335780919154, 70.00779233799265455 ) ) ;
#11790 = DIRECTION ( 'NONE',  ( -0.1733269559585509378, 0.000000000000000000, -0.9848643390529188135 ) ) ;
#11791 = CARTESIAN_POINT ( 'NONE',  ( 40.52078840805428683, -2.613682088886105870, 70.60699637195608602 ) ) ;
#11792 = LINE ( 'NONE', #9725, #19245 ) ;
#11793 = ORIENTED_EDGE ( 'NONE', *, *, #14530, .T. ) ;
#11794 = EDGE_LOOP ( 'NONE', ( #20504, #22652, #56, #10154 ) ) ;
#11795 = APPLICATION_CONTEXT ( 'automotive_design' ) ;
#11796 = DIRECTION ( 'NONE',  ( -1.734723475976814737E-16, 1.000000000000000000, -3.491481338843135327E-15 ) ) ;
#11797 = LINE ( 'NONE', #7544, #21673 ) ;
#11798 = CARTESIAN_POINT ( 'NONE',  ( 37.33957961208645315, -23.80384086642191122, 69.94417936956671156 ) ) ;
#11799 = CARTESIAN_POINT ( 'NONE',  ( 32.81606138205700773, 44.92314894770294131, 81.17823623207320338 ) ) ;
#11800 = VERTEX_POINT ( 'NONE', #5110 ) ;
#11801 = DIRECTION ( 'NONE',  ( 1.000000000000000000, 1.734723475976804876E-16, -1.734723475976814737E-16 ) ) ;
#11802 = CARTESIAN_POINT ( 'NONE',  ( 42.96606138205698500, -6.570990706613058840, -2.335727660491067503 ) ) ;
#11803 = PLANE ( 'NONE',  #20865 ) ;
#11804 = EDGE_CURVE ( 'NONE', #9092, #10854, #834, .T. ) ;
#11805 = CARTESIAN_POINT ( 'NONE',  ( 37.69225076346193504, -3.803840866421912992, 70.42958956619168021 ) ) ;
#11806 = ADVANCED_FACE ( 'NONE', ( #22489 ), #12971, .T. ) ;
#11807 = ORIENTED_EDGE ( 'NONE', *, *, #1948, .T. ) ;
#11808 = DIRECTION ( 'NONE',  ( 0.000000000000000000, -1.000000000000000000, 2.999999999999999839E-15 ) ) ;
#11809 = ORIENTED_EDGE ( 'NONE', *, *, #19821, .F. ) ;
#11810 = EDGE_LOOP ( 'NONE', ( #2967, #20673, #13703, #974 ) ) ;
#11811 = CARTESIAN_POINT ( 'NONE',  ( 32.31606138205700063, 10.62769494289597993, 68.29765714199933768 ) ) ;
#11812 = CARTESIAN_POINT ( 'NONE',  ( 37.69225076346193504, -11.81368208888610205, 72.33091598616826445 ) ) ;
#11813 = CARTESIAN_POINT ( 'NONE',  ( 37.25260217561390874, -9.613682088886102761, 71.78268878715394408 ) ) ;
#11814 = ORIENTED_EDGE ( 'NONE', *, *, #21150, .T. ) ;
#11815 = ORIENTED_EDGE ( 'NONE', *, *, #12407, .F. ) ;
#11816 = DIRECTION ( 'NONE',  ( 1.000000000000000000, -0.000000000000000000, -0.000000000000000000 ) ) ;
#11817 = DIRECTION ( 'NONE',  ( 1.000000000000000000, 0.000000000000000000, 0.000000000000000000 ) ) ;
#11818 = ORIENTED_EDGE ( 'NONE', *, *, #7366, .F. ) ;
#11819 = EDGE_CURVE ( 'NONE', #8848, #9377, #11027, .T. ) ;
#11820 = LINE ( 'NONE', #5883, #3746 ) ;
#11821 = CARTESIAN_POINT ( 'NONE',  ( 39.75915168707251723, -14.90384086642191086, 72.49904802271738902 ) ) ;
#11822 = VECTOR ( 'NONE', #21315, 1000.000000000000000 ) ;
#11823 = VECTOR ( 'NONE', #268, 1000.000000000000000 ) ;
#11824 = CARTESIAN_POINT ( 'NONE',  ( 38.31606138205700063, -22.22127907754186893, 75.81001292736998209 ) ) ;
#11825 = CARTESIAN_POINT ( 'NONE',  ( 45.81606138205697221, -6.210967385200538260, -3.065230171572501661 ) ) ;
#11826 = CARTESIAN_POINT ( 'NONE',  ( 38.63098279924288647, -16.91368208888609814, 70.22690120949090442 ) ) ;
#11827 = ORIENTED_EDGE ( 'NONE', *, *, #12974, .T. ) ;
#11828 = ORIENTED_EDGE ( 'NONE', *, *, #4831, .F. ) ;
#11829 = DIRECTION ( 'NONE',  ( 2.690219486203388234E-15, -0.8967398287344627850, -0.4425581086832399147 ) ) ;
#11830 = CARTESIAN_POINT ( 'NONE',  ( 36.64852494920107517, -15.41368208888610525, 70.89533451361947414 ) ) ;
#11831 = EDGE_CURVE ( 'NONE', #16347, #22563, #20559, .T. ) ;
#11832 = LINE ( 'NONE', #4348, #14321 ) ;
#11833 = DIRECTION ( 'NONE',  ( -1.000000000000000000, 0.000000000000000000, 0.000000000000000000 ) ) ;
#11834 = CARTESIAN_POINT ( 'NONE',  ( 40.14115730948191185, -28.51368208888610667, 71.32335560751958781 ) ) ;
#11835 = CARTESIAN_POINT ( 'NONE',  ( 43.31606138205700063, -35.70002751211045933, 71.94742330197156832 ) ) ;
#11836 = VECTOR ( 'NONE', #11034, 1000.000000000000000 ) ;
#11837 = CARTESIAN_POINT ( 'NONE',  ( 44.31606138205700063, -21.26162886970023536, 44.16441745890789150 ) ) ;
#11838 = AXIS2_PLACEMENT_3D ( 'NONE', #15606, #1816, #7383 ) ;
#11839 = VECTOR ( 'NONE', #19606, 1000.000000000000000 ) ;
#11840 = EDGE_LOOP ( 'NONE', ( #16477, #24634, #10489, #4733 ) ) ;
#11841 = CARTESIAN_POINT ( 'NONE',  ( 33.31606138205700773, -4.357181138186130731, 81.40610939240430355 ) ) ;
#11842 = ORIENTED_EDGE ( 'NONE', *, *, #9957, .T. ) ;
#11843 = ORIENTED_EDGE ( 'NONE', *, *, #15075, .T. ) ;
#11844 = CARTESIAN_POINT ( 'NONE',  ( 36.07789103942399578, -6.203840866421916900, 72.05058123536544201 ) ) ;
#11845 = ORIENTED_EDGE ( 'NONE', *, *, #5213, .F. ) ;
#11846 = DIRECTION ( 'NONE',  ( 0.000000000000000000, 0.7540134720837717852, 0.6568589528324746407 ) ) ;
#11847 = CARTESIAN_POINT ( 'NONE',  ( 37.80618814713140097, -13.91368208888610347, 73.13360434286903455 ) ) ;
#11848 = VERTEX_POINT ( 'NONE', #16558 ) ;
#11849 = CYLINDRICAL_SURFACE ( 'NONE', #21915, 10.00000000000000000 ) ;
#11850 = SURFACE_SIDE_STYLE ('',( #19690 ) ) ;
#11851 = CARTESIAN_POINT ( 'NONE',  ( 40.55423172469004811, -12.41368208888610525, 72.05058123536544201 ) ) ;
#11852 = COLOUR_RGB ( '', 0.09019608, 0.27058824, 0.51372549) ;
#11853 = EDGE_LOOP ( 'NONE', ( #8498, #4393, #21970, #6696 ) ) ;
#11854 = ADVANCED_FACE ( 'NONE', ( #10906 ), #3286, .T. ) ;
#11855 = DIRECTION ( 'NONE',  ( 1.734723475976814737E-16, -1.000000000000000000, 3.491481338843135327E-15 ) ) ;
#11856 = ADVANCED_FACE ( 'NONE', ( #7031 ), #1223, .F. ) ;
#11857 = AXIS2_PLACEMENT_3D ( 'NONE', #23358, #3650, #13456 ) ;
#11858 = VECTOR ( 'NONE', #16983, 1000.000000000000000 ) ;
#11859 = CARTESIAN_POINT ( 'NONE',  ( 41.31606138205700063, 8.104266321858618838, 55.82104096753806033 ) ) ;
#11860 = ADVANCED_FACE ( 'NONE', ( #7166 ), #5228, .T. ) ;
#11861 = CARTESIAN_POINT ( 'NONE',  ( 36.81465384343994884, 41.67000142393845152, 79.37823623207322044 ) ) ;
#11862 = LINE ( 'NONE', #18159, #11507 ) ;
#11863 = LINE ( 'NONE', #12239, #2617 ) ;
#11864 = CARTESIAN_POINT ( 'NONE',  ( 37.31647492878124694, -10.30384086642191122, 72.03616607671141026 ) ) ;
#11865 = CARTESIAN_POINT ( 'NONE',  ( 38.26194895904383486, -29.01368208888610312, 70.24448340153875847 ) ) ;
#11866 = EDGE_LOOP ( 'NONE', ( #24262, #18076, #21530, #20066 ) ) ;
#11867 = FACE_OUTER_BOUND ( 'NONE', #10689, .T. ) ;
#11868 = EDGE_CURVE ( 'NONE', #10765, #24723, #13092, .T. ) ;
#11869 = DIRECTION ( 'NONE',  ( 0.000000000000000000, 0.000000000000000000, 1.000000000000000000 ) ) ;
#11870 = ORIENTED_EDGE ( 'NONE', *, *, #7346, .T. ) ;
#11871 = AXIS2_PLACEMENT_3D ( 'NONE', #4514, #14185, #8256 ) ;
#11872 = ORIENTED_EDGE ( 'NONE', *, *, #5014, .T. ) ;
#11873 = CARTESIAN_POINT ( 'NONE',  ( 40.33642880535521869, -23.30384086642191477, 69.98269868914866265 ) ) ;
#11874 = VECTOR ( 'NONE', #22521, 1000.000000000000114 ) ;
#11875 = CARTESIAN_POINT ( 'NONE',  ( 38.37017380507020192, -22.01368208888610312, 72.51602215082118619 ) ) ;
#11876 = CARTESIAN_POINT ( 'NONE',  ( 36.07789103942398867, -3.413682088886104804, 70.70992431699450265 ) ) ;
#11877 = ORIENTED_EDGE ( 'NONE', *, *, #1826, .T. ) ;
#11878 = DIRECTION ( 'NONE',  ( 1.000000000000000000, 0.000000000000000000, 0.000000000000000000 ) ) ;
#11879 = CARTESIAN_POINT ( 'NONE',  ( 37.60469502381300799, -0.4038408664219124145, 72.26730301774236409 ) ) ;
#11880 = ORIENTED_EDGE ( 'NONE', *, *, #17520, .F. ) ;
#11881 = CARTESIAN_POINT ( 'NONE',  ( 59.50607210797845426, 32.97469880962110267, 83.30501292736985874 ) ) ;
#11882 = LINE ( 'NONE', #2440, #3009 ) ;
#11883 = CARTESIAN_POINT ( 'NONE',  ( 36.98690846071097127, -5.803840866421911215, 69.45876917294177133 ) ) ;
#11884 = B_SPLINE_CURVE_WITH_KNOTS ( 'NONE', 3,
 ( #16353, #14058, #14436, #19854 ),
 .UNSPECIFIED., .F., .F.,
 ( 4, 4 ),
 ( 0.000000000000000000, 0.9997489389489839784 ),
 .UNSPECIFIED. ) ;
#11885 = PLANE ( 'NONE',  #2041 ) ;
#11886 = FILL_AREA_STYLE_COLOUR ( '', #13656 ) ;
#11887 = CARTESIAN_POINT ( 'NONE',  ( 36.80608444377001121, -13.31368208888609672, 70.35351908239857721 ) ) ;
#11888 = DIRECTION ( 'NONE',  ( -7.071067811865491110E-16, 0.9008287146801832179, -0.4341746501209495790 ) ) ;
#11889 = CARTESIAN_POINT ( 'NONE',  ( 37.33957961208646736, -23.81368208888611093, 72.81632618279320468 ) ) ;
#11890 = LINE ( 'NONE', #16110, #8656 ) ;
#11891 = CARTESIAN_POINT ( 'NONE',  ( 38.26194895904384907, -4.603840866421914590, 73.11602215082118050 ) ) ;
#11892 = DIRECTION ( 'NONE',  ( 0.000000000000000000, -0.3299742535180974490, 0.9439899321577398528 ) ) ;
#11893 = CARTESIAN_POINT ( 'NONE',  ( 37.33957961208646736, -17.81368208888611093, 72.81632618279321889 ) ) ;
#11894 = CARTESIAN_POINT ( 'NONE',  ( 33.31606138205700773, 3.172506336381830661, 12.50058896911730066 ) ) ;
#11895 = ADVANCED_FACE ( 'NONE', ( #6783 ), #2893, .T. ) ;
#11896 = COLOUR_RGB ( '', 0.08235294, 0.09019608, 0.10196078) ;
#11897 = CARTESIAN_POINT ( 'NONE',  ( 36.64852494920107517, -18.20384086642191335, 71.86517103874048473 ) ) ;
#11898 = DIRECTION ( 'NONE',  ( 1.000000000000000000, 2.490066548941357423E-15, 1.228895056384527422E-15 ) ) ;
#11899 = CARTESIAN_POINT ( 'NONE',  ( 39.29254315202756231, -14.81368208888610205, 69.94417936956672577 ) ) ;
#11900 = ORIENTED_EDGE ( 'NONE', *, *, #2520, .F. ) ;
#11901 = CARTESIAN_POINT ( 'NONE',  ( 40.33642880535524000, -20.31368208888610738, 72.77780686321126780 ) ) ;
#11902 = ORIENTED_EDGE ( 'NONE', *, *, #333, .T. ) ;
#11903 = CARTESIAN_POINT ( 'NONE',  ( 40.71606138205696368, 0.5799492015812739432, -3.145019409304214530 ) ) ;
#11904 = CARTESIAN_POINT ( 'NONE',  ( 36.31606138205702194, -20.30191568716149320, 23.22716926412510219 ) ) ;
#11905 = CARTESIAN_POINT ( 'NONE',  ( 39.02742774030101458, -21.40384086642191619, 70.49320253461759478 ) ) ;
#11906 = VECTOR ( 'NONE', #7003, 1000.000000000000114 ) ;
#11907 = ORIENTED_EDGE ( 'NONE', *, *, #24135, .T. ) ;
#11908 = ORIENTED_EDGE ( 'NONE', *, *, #22789, .F. ) ;
#11909 = CARTESIAN_POINT ( 'NONE',  ( 39.62003278564551323, -28.88720382805528430, 70.76953470883664465 ) ) ;
#11910 = B_SPLINE_CURVE_WITH_KNOTS ( 'NONE', 3,
 ( #20342, #2673, #2542, #10044, #12117, #10426, #5259, #20461 ),
 .UNSPECIFIED., .F., .F.,
 ( 4, 2, 2, 4 ),
 ( 0.0001628760028480823424, 0.0003078672859939987996, 0.0004528585691399152568, 0.0007428411354317482253 ),
 .UNSPECIFIED. ) ;
#11911 = DIRECTION ( 'NONE',  ( 4.336808689942074435E-17, -1.000000000000000000, 3.491481338843135327E-15 ) ) ;
#11912 = DIRECTION ( 'NONE',  ( -1.000000000000000000, -1.000000000000000078E-15, 0.000000000000000000 ) ) ;
#11913 = CARTESIAN_POINT ( 'NONE',  ( 39.75915168707251723, -0.9038408664219161892, 72.49904802271740323 ) ) ;
#11914 = AXIS2_PLACEMENT_3D ( 'NONE', #18657, #16330, #24437 ) ;
#11915 = PRESENTATION_STYLE_ASSIGNMENT (( #1967 ) ) ;
#11916 = CARTESIAN_POINT ( 'NONE',  ( 36.98690846071097837, 0.1863179111138910382, 73.30173637941818754 ) ) ;
#11917 = DIRECTION ( 'NONE',  ( 0.000000000000000000, -1.000000000000000000, 4.625929269271485322E-15 ) ) ;
#11918 = ORIENTED_EDGE ( 'NONE', *, *, #14980, .T. ) ;
#11919 = VECTOR ( 'NONE', #12123, 1000.000000000000000 ) ;
#11920 = ORIENTED_EDGE ( 'NONE', *, *, #21669, .F. ) ;
#11921 = CARTESIAN_POINT ( 'NONE',  ( 31.91606138205697363, -3.929900956088018038, -7.102449327239662935 ) ) ;
#11922 = CARTESIAN_POINT ( 'NONE',  ( 43.31606138205700063, 7.166937456968672571, 6.752152658007350539 ) ) ;
#11923 = CARTESIAN_POINT ( 'NONE',  ( 36.64852494920107517, -20.20384086642191335, 71.86517103874048473 ) ) ;
#11924 =( LENGTH_UNIT ( ) NAMED_UNIT ( * ) SI_UNIT ( .MILLI., .METRE. ) );
#11925 = CARTESIAN_POINT ( 'NONE',  ( 32.81606138205700773, -24.55876147765400574, 72.80501292737008612 ) ) ;
#11926 = CIRCLE ( 'NONE', #17248, 2.500000000000002220 ) ;
#11927 = ORIENTED_EDGE ( 'NONE', *, *, #14894, .F. ) ;
#11928 = PLANE ( 'NONE',  #20516 ) ;
#11929 = EDGE_CURVE ( 'NONE', #15369, #22901, #6904, .T. ) ;
#11930 = CARTESIAN_POINT ( 'NONE',  ( 31.81606138205700418, -27.70293563151089700, 74.66612024218476051 ) ) ;
#11931 = EDGE_LOOP ( 'NONE', ( #15665, #7206, #14397, #4000 ) ) ;
#11932 = CARTESIAN_POINT ( 'NONE',  ( 38.26194895904384197, -8.603840866421911926, 72.51602215082118619 ) ) ;
#11933 = CIRCLE ( 'NONE', #18928, 0.5000000000000008882 ) ;
#11934 = CARTESIAN_POINT ( 'NONE',  ( 44.06606138205700063, 40.39281886181299797, 83.30501292736984453 ) ) ;
#11935 = ORIENTED_EDGE ( 'NONE', *, *, #2233, .T. ) ;
#11936 = VECTOR ( 'NONE', #20382, 1000.000000000000000 ) ;
#11937 = LINE ( 'NONE', #18111, #18969 ) ;
#11938 = ORIENTED_EDGE ( 'NONE', *, *, #11008, .F. ) ;
#11939 = EDGE_LOOP ( 'NONE', ( #23017, #6292, #17479, #2116 ) ) ;
#11940 = LINE ( 'NONE', #9498, #22519 ) ;
#11941 = CIRCLE ( 'NONE', #2832, 1.550000000000002709 ) ;
#11942 = CARTESIAN_POINT ( 'NONE',  ( 38.73920764526925353, -10.11368208888610276, 72.49843995877331793 ) ) ;
#11943 = CARTESIAN_POINT ( 'NONE',  ( 37.60469502381300089, -5.213682088886100630, 70.49320253461759478 ) ) ;
#11944 = EDGE_LOOP ( 'NONE', ( #3334, #17861, #3054, #16445 ) ) ;
#11945 = VERTEX_POINT ( 'NONE', #18756 ) ;
#11946 = CARTESIAN_POINT ( 'NONE',  ( 47.81606138205695800, 0.8576245772853805516, -1.570935883000508460 ) ) ;
#11947 = DIRECTION ( 'NONE',  ( -5.047295537021760406E-31, 1.000000000000000000, -3.491481338843135327E-15 ) ) ;
#11948 = ORIENTED_EDGE ( 'NONE', *, *, #16022, .T. ) ;
#11949 = DIRECTION ( 'NONE',  ( 6.109829820097539848E-16, -0.6595716529892418079, 0.7516416929448760387 ) ) ;
#11950 = AXIS2_PLACEMENT_3D ( 'NONE', #23584, #13549, #2066 ) ;
#11951 = CARTESIAN_POINT ( 'NONE',  ( 36.68196826583682935, -16.00384086642191050, 70.79240656858107172 ) ) ;
#11952 = ADVANCED_FACE ( 'NONE', ( #4727, #20433, #3790 ), #15138, .F. ) ;
#11953 = EDGE_CURVE ( 'NONE', #22382, #981, #15513, .T. ) ;
#11954 = CARTESIAN_POINT ( 'NONE',  ( 43.24475484328152675, -1.357181138186998925, 80.05501292736997243 ) ) ;
#11955 = CYLINDRICAL_SURFACE ( 'NONE', #6299, 3.999999999999899636 ) ;
#11956 = CARTESIAN_POINT ( 'NONE',  ( 37.25260217561390874, -19.61368208888610098, 71.78268878715392987 ) ) ;
#11957 = EDGE_CURVE ( 'NONE', #3232, #5590, #13226, .T. ) ;
#11958 = ORIENTED_EDGE ( 'NONE', *, *, #18218, .T. ) ;
#11959 = ADVANCED_FACE ( 'NONE', ( #21317 ), #24905, .F. ) ;
#11960 = ORIENTED_EDGE ( 'NONE', *, *, #23090, .F. ) ;
#11961 = PLANE ( 'NONE',  #14128 ) ;
#11962 = VECTOR ( 'NONE', #3491, 1000.000000000000114 ) ;
#11963 = CARTESIAN_POINT ( 'NONE',  ( 38.82593461698262871, -12.91368208888610170, 69.62690120949091011 ) ) ;
#11964 = PLANE ( 'NONE',  #1966 ) ;
#11965 = CYLINDRICAL_SURFACE ( 'NONE', #3406, 2.000000000000001776 ) ;
#11966 = VECTOR ( 'NONE', #427, 1000.000000000000000 ) ;
#11967 = CARTESIAN_POINT ( 'NONE',  ( 32.31606138205700063, 10.29926546647973851, 68.67466387804121553 ) ) ;
#11968 = CARTESIAN_POINT ( 'NONE',  ( 40.02576592390014554, -29.10876147765401001, 70.31011966505063526 ) ) ;
#11969 = EDGE_CURVE ( 'NONE', #643, #16610, #24365, .T. ) ;
#11970 = ADVANCED_FACE ( 'NONE', ( #19382 ), #5863, .T. ) ;
#11971 = DIRECTION ( 'NONE',  ( -0.1733269559585477460, -5.551115123125804790E-15, -0.9848643390529193686 ) ) ;
#11972 = LINE ( 'NONE', #2523, #14316 ) ;
#11973 = EDGE_LOOP ( 'NONE', ( #2161, #4579, #13763, #8789 ) ) ;
#11974 = FACE_OUTER_BOUND ( 'NONE', #7650, .T. ) ;
#11975 = ORIENTED_EDGE ( 'NONE', *, *, #16964, .T. ) ;
#11976 = EDGE_LOOP ( 'NONE', ( #21178, #5775, #8095, #18343, #6190 ) ) ;
#11977 = CARTESIAN_POINT ( 'NONE',  ( 40.52078840805429394, -5.003840866421915834, 72.15350918040385864 ) ) ;
#11978 = CIRCLE ( 'NONE', #21003, 2.500000000000002220 ) ;
#11979 = ORIENTED_EDGE ( 'NONE', *, *, #23552, .T. ) ;
#11980 = EDGE_CURVE ( 'NONE', #19667, #4130, #13722, .T. ) ;
#11981 = DIRECTION ( 'NONE',  ( 1.734723475976814737E-16, -1.000000000000000000, 3.491481338843135327E-15 ) ) ;
#11982 = CARTESIAN_POINT ( 'NONE',  ( 39.29254315202756231, -8.813682088886100274, 69.94417936956673998 ) ) ;
#11983 = VECTOR ( 'NONE', #24311, 1000.000000000000000 ) ;
#11984 = ORIENTED_EDGE ( 'NONE', *, *, #18533, .F. ) ;
#11985 = CARTESIAN_POINT ( 'NONE',  ( 40.31606138205701484, -19.34838015056930161, 26.94402965816085072 ) ) ;
#11986 = CARTESIAN_POINT ( 'NONE',  ( 36.98690846071097837, -15.81368208888610916, 73.30173637941818754 ) ) ;
#11987 = ADVANCED_BREP_SHAPE_REPRESENTATION ( '', ( #322, #2000 ), #3041 ) ;
#11988 = CARTESIAN_POINT ( 'NONE',  ( 33.31606138205700773, -5.204193249396280585, 82.80501292736992980 ) ) ;
#11989 = LINE ( 'NONE', #19954, #4629 ) ;
#11990 = EDGE_LOOP ( 'NONE', ( #16860, #13892, #24196, #11377 ) ) ;
#11991 = CARTESIAN_POINT ( 'NONE',  ( 43.81606138205700063, 41.44123852234595518, 61.30501292736988006 ) ) ;
#11992 = VECTOR ( 'NONE', #21720, 1000.000000000000114 ) ;
#11993 = CARTESIAN_POINT ( 'NONE',  ( 38.31606138205700063, -1.054793099133682244, 61.76760556592023477 ) ) ;
#11994 = CARTESIAN_POINT ( 'NONE',  ( 39.81746892067405952, 41.90149715599300606, 79.37823623207322044 ) ) ;
#11995 = LINE ( 'NONE', #19833, #353 ) ;
#11996 = CARTESIAN_POINT ( 'NONE',  ( 38.26194895904383486, -27.01368208888609956, 70.24448340153875847 ) ) ;
#11997 = ORIENTED_EDGE ( 'NONE', *, *, #13973, .T. ) ;
#11998 = LINE ( 'NONE', #13661, #1217 ) ;
#11999 = DIRECTION ( 'NONE',  ( -1.000000000000000000, -3.046270958365671426E-15, 5.272995181423179347E-17 ) ) ;
#12000 = VERTEX_POINT ( 'NONE', #19516 ) ;
#12001 = ORIENTED_EDGE ( 'NONE', *, *, #24012, .F. ) ;
#12002 = CARTESIAN_POINT ( 'NONE',  ( 39.12911128074872380, -21.50384086642191406, 69.06206559358665231 ) ) ;
#12003 = CARTESIAN_POINT ( 'NONE',  ( 37.12184278917507640, -21.51368208888609956, 71.43714994484034264 ) ) ;
#12004 = B_SPLINE_SURFACE_WITH_KNOTS ( 'NONE', 1, 3, ( 
 ( #14413, #14539, #20848, #4748 ),
 ( #7063, #24178, #8749, #12623 ),
 ( #998, #12751, #14656, #6552 ) ),
 .UNSPECIFIED., .F., .F., .F.,
 ( 2, 1, 2 ),
 ( 4, 4 ),
 ( -0.01000000000000000021, 0.000000000000000000, 1.000000000000000000 ),
 ( 0.000000000000000000, 1.000000000000000000 ),
 .UNSPECIFIED. ) ;
#12005 = CARTESIAN_POINT ( 'NONE',  ( 39.98359781491296161, -28.41368208888610525, 71.86517103874045631 ) ) ;
#12006 = CARTESIAN_POINT ( 'NONE',  ( 31.81606138205700418, -34.55876147765401640, 70.30501292737011454 ) ) ;
#12007 = CARTESIAN_POINT ( 'NONE',  ( 37.38336156205273397, 0.09615913357808798800, 70.63227792289248441 ) ) ;
#12008 =( NAMED_UNIT ( * ) PLANE_ANGLE_UNIT ( ) SI_UNIT ( $, .RADIAN. ) );
#12009 = ORIENTED_EDGE ( 'NONE', *, *, #12027, .T. ) ;
#12010 = LINE ( 'NONE', #23826, #5984 ) ;
#12011 = CARTESIAN_POINT ( 'NONE',  ( 40.64099152588523367, -8.607181138186998481, 88.30501292736998664 ) ) ;
#12012 = CARTESIAN_POINT ( 'NONE',  ( 39.64521430340305841, -2.803840866421918765, 73.30173637941818754 ) ) ;
#12013 = VECTOR ( 'NONE', #15535, 1000.000000000000000 ) ;
#12014 = DIRECTION ( 'NONE',  ( -1.123589211228918605E-15, 0.4425581086832399147, -0.8967398287344627850 ) ) ;
#12015 = DIRECTION ( 'NONE',  ( 0.000000000000000000, 0.5706330172266930179, -0.8212051873014202252 ) ) ;
#12016 = CARTESIAN_POINT ( 'NONE',  ( 39.29254315202756231, -4.813682088886099386, 69.94417936956673998 ) ) ;
#12017 = DIRECTION ( 'NONE',  ( 0.000000000000000000, 0.3299742535180963943, -0.9439899321577402969 ) ) ;
#12018 = STYLED_ITEM ( 'NONE', ( #9322 ), #17206 ) ;
#12019 = CARTESIAN_POINT ( 'NONE',  ( 39.82603832034401847, -26.31368208888610738, 72.40698646996131060 ) ) ;
#12020 = CARTESIAN_POINT ( 'NONE',  ( 46.91606138205695231, -23.19619402982945644, 47.16846523730003327 ) ) ;
#12021 = CARTESIAN_POINT ( 'NONE',  ( 37.80618814713138676, 0.2961591335780937584, 69.62690120949092432 ) ) ;
#12022 = DIRECTION ( 'NONE',  ( -1.000000000000000000, -1.000000000000000078E-15, 0.000000000000000000 ) ) ;
#12023 = CARTESIAN_POINT ( 'NONE',  ( 38.93987200065210175, -24.80384086642191477, 72.33091598616823603 ) ) ;
#12024 = CARTESIAN_POINT ( 'NONE',  ( 39.95015449827720744, -10.61368208888610631, 70.79240656858107172 ) ) ;
#12025 = CARTESIAN_POINT ( 'NONE',  ( 43.31606138205700063, -10.93995761290683255, 80.99653337025984001 ) ) ;
#12026 = CIRCLE ( 'NONE', #20230, 3.000000000000000888 ) ;
#12027 = EDGE_CURVE ( 'NONE', #9092, #18170, #1594, .T. ) ;
#12028 = CARTESIAN_POINT ( 'NONE',  ( 39.98359781491296161, -13.20384086642191157, 70.89533451361945993 ) ) ;
#12029 = CARTESIAN_POINT ( 'NONE',  ( 40.31606138205700773, 37.94123852234599781, 75.30501292736988717 ) ) ;
#12030 = VECTOR ( 'NONE', #4984, 1000.000000000000000 ) ;
#12031 = CARTESIAN_POINT ( 'NONE',  ( 36.87297107704152666, -9.713682088886107735, 72.49904802271743165 ) ) ;
#12032 = ORIENTED_EDGE ( 'NONE', *, *, #18714, .T. ) ;
#12033 = CARTESIAN_POINT ( 'NONE',  ( 39.02088643472237095, -24.91368208888610170, 69.02690120949091579 ) ) ;
#12034 = ORIENTED_EDGE ( 'NONE', *, *, #13277, .F. ) ;
#12035 = FACE_OUTER_BOUND ( 'NONE', #2426, .T. ) ;
#12036 = CARTESIAN_POINT ( 'NONE',  ( 38.93987200065210175, -18.80384086642191122, 72.33091598616826445 ) ) ;
#12037 = VERTEX_POINT ( 'NONE', #25415 ) ;
#12038 = ORIENTED_EDGE ( 'NONE', *, *, #4522, .T. ) ;
#12039 = CARTESIAN_POINT ( 'NONE',  ( 39.60564227155354189, -28.80873119892454071, 70.65162531128912349 ) ) ;
#12040 = DIRECTION ( 'NONE',  ( 0.000000000000000000, 2.999999999999999839E-15, 1.000000000000000000 ) ) ;
#12041 = CARTESIAN_POINT ( 'NONE',  ( 36.11133435605973574, -22.00384086642191761, 70.60699637195608602 ) ) ;
#12042 = CARTESIAN_POINT ( 'NONE',  ( 36.31606138205700063, -13.04008168869994932, 21.66778101221729713 ) ) ;
#12043 = CARTESIAN_POINT ( 'NONE',  ( 36.80608444377001121, -27.31368208888610383, 70.35351908239857721 ) ) ;
#12044 = EDGE_CURVE ( 'NONE', #18988, #12980, #7799, .T. ) ;
#12045 = CARTESIAN_POINT ( 'NONE',  ( 45.81606138205706458, -34.55876147768182705, 70.30501292735635843 ) ) ;
#12046 = AXIS2_PLACEMENT_3D ( 'NONE', #12341, #8592, #20317 ) ;
#12047 = EDGE_LOOP ( 'NONE', ( #21140, #8913, #14740, #10951 ) ) ;
#12048 = ORIENTED_EDGE ( 'NONE', *, *, #5750, .F. ) ;
#12049 = CARTESIAN_POINT ( 'NONE',  ( 35.64099152588522657, -8.167181138186998979, 78.30501292736998664 ) ) ;
#12050 = DIRECTION ( 'NONE',  ( -1.000000000000000000, 4.930380657631319405E-32, 1.734723475976804876E-16 ) ) ;
#12051 = VECTOR ( 'NONE', #824, 1000.000000000000000 ) ;
#12052 = CARTESIAN_POINT ( 'NONE',  ( 37.33957961208645315, -21.80384086642190766, 69.94417936956672577 ) ) ;
#12053 = PLANE ( 'NONE',  #14137 ) ;
#12054 = ORIENTED_EDGE ( 'NONE', *, *, #336, .F. ) ;
#12055 = CARTESIAN_POINT ( 'NONE',  ( 36.31606138205700063, -11.51539968388052060, 18.41550321377400934 ) ) ;
#12056 = AXIS2_PLACEMENT_3D ( 'NONE', #3086, #22920, #885 ) ;
#12057 = VECTOR ( 'NONE', #3050, 1000.000000000000000 ) ;
#12058 = CARTESIAN_POINT ( 'NONE',  ( 43.81606138205700063, -34.55876147765401640, 70.30501292737011454 ) ) ;
#12059 = CARTESIAN_POINT ( 'NONE',  ( 37.31647492878124694, -2.303840866421911215, 72.03616607671141026 ) ) ;
#12060 = DIRECTION ( 'NONE',  ( 1.000000000000000000, 1.115287202090205222E-30, -1.734723475976805122E-15 ) ) ;
#12061 = VERTEX_POINT ( 'NONE', #1718 ) ;
#12062 = LINE ( 'NONE', #18234, #9112 ) ;
#12063 = ORIENTED_EDGE ( 'NONE', *, *, #20664, .T. ) ;
#12064 = ORIENTED_EDGE ( 'NONE', *, *, #3113, .F. ) ;
#12065 = VECTOR ( 'NONE', #3660, 1000.000000000000000 ) ;
#12066 = DIRECTION ( 'NONE',  ( 1.000000000000000000, 0.000000000000000000, 0.000000000000000000 ) ) ;
#12067 = CARTESIAN_POINT ( 'NONE',  ( 38.93987200065208754, -8.813682088886096722, 70.42958956619168021 ) ) ;
#12068 = CARTESIAN_POINT ( 'NONE',  ( 37.38336156205274818, -7.713682088886103294, 72.12822762946751709 ) ) ;
#12069 = EDGE_LOOP ( 'NONE', ( #14502, #5879, #13235, #702 ) ) ;
#12070 = ORIENTED_EDGE ( 'NONE', *, *, #13143, .T. ) ;
#12071 = LINE ( 'NONE', #23770, #10731 ) ;
#12072 = VECTOR ( 'NONE', #22318, 1000.000000000000000 ) ;
#12073 = FACE_OUTER_BOUND ( 'NONE', #3774, .T. ) ;
#12074 = CARTESIAN_POINT ( 'NONE',  ( 40.56606138205700773, 6.004618353093779781, 2.291321535809666354 ) ) ;
#12075 = CARTESIAN_POINT ( 'NONE',  ( 37.69796330110505522, -8.503840866421915834, 73.09843995877331224 ) ) ;
#12076 = CARTESIAN_POINT ( 'NONE',  ( 42.56606138205700063, -40.62725863591898445, 68.52362519861142687 ) ) ;
#12077 = CIRCLE ( 'NONE', #933, 0.7500000000000031086 ) ;
#12078 = EDGE_CURVE ( 'NONE', #20194, #4468, #6301, .T. ) ;
#12079 = DIRECTION ( 'NONE',  ( 1.000000000000000000, 2.065146995210479765E-16, -1.734723475976814737E-16 ) ) ;
#12080 = ORIENTED_EDGE ( 'NONE', *, *, #6413, .T. ) ;
#12081 = ORIENTED_EDGE ( 'NONE', *, *, #812, .T. ) ;
#12082 = LINE ( 'NONE', #4471, #7956 ) ;
#12083 = CARTESIAN_POINT ( 'NONE',  ( 37.80618814713140097, -9.913682088886107024, 73.13360434286904876 ) ) ;
#12084 = AXIS2_PLACEMENT_3D ( 'NONE', #8835, #16673, #24506 ) ;
#12085 = CARTESIAN_POINT ( 'NONE',  ( 35.64099152588522657, 0.3928188618129990761, 82.55501292736997243 ) ) ;
#12086 = CIRCLE ( 'NONE', #12512, 4.000000000000003553 ) ;
#12087 = LINE ( 'NONE', #2648, #924 ) ;
#12088 = DIRECTION ( 'NONE',  ( -1.734723475976804876E-16, -3.491481338843135327E-15, -1.000000000000000000 ) ) ;
#12089 = CARTESIAN_POINT ( 'NONE',  ( 36.31606138205699352, -10.17000407126884731, 36.59108960988216808 ) ) ;
#12090 = AXIS2_PLACEMENT_3D ( 'NONE', #17802, #6328, #10073 ) ;
#12091 = CARTESIAN_POINT ( 'NONE',  ( 40.31606138205700773, -5.204193249396356968, 72.80501292736992980 ) ) ;
#12092 = CARTESIAN_POINT ( 'NONE',  ( 46.81606138205706458, -34.55876147768182705, 70.30501292735635843 ) ) ;
#12093 = EDGE_CURVE ( 'NONE', #2564, #24591, #3418, .T. ) ;
#12094 = ORIENTED_EDGE ( 'NONE', *, *, #24060, .F. ) ;
#12095 = EDGE_CURVE ( 'NONE', #16335, #3835, #11232, .T. ) ;
#12096 = VECTOR ( 'NONE', #18344, 1000.000000000000000 ) ;
#12097 = DIRECTION ( 'NONE',  ( 5.664403186863039509E-16, 3.000000000000000628E-15, 1.000000000000000000 ) ) ;
#12098 = ORIENTED_EDGE ( 'NONE', *, *, #16964, .F. ) ;
#12099 = EDGE_CURVE ( 'NONE', #5726, #13134, #19257, .T. ) ;
#12100 = VERTEX_POINT ( 'NONE', #17087 ) ;
#12101 = CARTESIAN_POINT ( 'NONE',  ( 43.31606138205700063, -27.17722769842920272, 59.42551550655435477 ) ) ;
#12102 = CARTESIAN_POINT ( 'NONE',  ( 36.29569395875881099, -6.303840866421917433, 72.77780686321129622 ) ) ;
#12103 = EDGE_CURVE ( 'NONE', #7176, #1142, #7671, .T. ) ;
#12104 = EDGE_CURVE ( 'NONE', #3683, #11458, #19140, .T. ) ;
#12105 = ORIENTED_EDGE ( 'NONE', *, *, #15849, .T. ) ;
#12106 = DIRECTION ( 'NONE',  ( 0.000000000000000000, -0.8967398287344631180, -0.4425581086832393041 ) ) ;
#12107 = CARTESIAN_POINT ( 'NONE',  ( 38.82593461698262871, -10.91368208888609992, 69.62690120949091011 ) ) ;
#12108 = CIRCLE ( 'NONE', #3444, 1.499999999999999778 ) ;
#12109 = ORIENTED_EDGE ( 'NONE', *, *, #4387, .T. ) ;
#12110 = DIRECTION ( 'NONE',  ( 1.000000000000000000, 0.000000000000000000, 0.000000000000000000 ) ) ;
#12111 = VECTOR ( 'NONE', #5276, 1000.000000000000114 ) ;
#12112 = EDGE_CURVE ( 'NONE', #19940, #4607, #11269, .T. ) ;
#12113 = CARTESIAN_POINT ( 'NONE',  ( 39.02088643472237095, -14.91368208888609992, 69.02690120949091579 ) ) ;
#12114 = ADVANCED_FACE ( 'NONE', ( #25292 ), #15266, .F. ) ;
#12115 = LINE ( 'NONE', #10422, #2436 ) ;
#12116 = CYLINDRICAL_SURFACE ( 'NONE', #25180, 0.4999999999999982792 ) ;
#12117 = CARTESIAN_POINT ( 'NONE',  ( 39.61922982725797482, -28.88282523147813663, 69.90442756104691568 ) ) ;
#12118 =( NAMED_UNIT ( * ) SI_UNIT ( $, .STERADIAN. ) SOLID_ANGLE_UNIT ( ) );
#12119 = CARTESIAN_POINT ( 'NONE',  ( 33.39768049593357091, 3.266176032039786570, 6.243079984136794991 ) ) ;
#12120 = VECTOR ( 'NONE', #7016, 1000.000000000000000 ) ;
#12121 = AXIS2_PLACEMENT_3D ( 'NONE', #18115, #310, #23887 ) ;
#12122 = LINE ( 'NONE', #7731, #18280 ) ;
#12123 = DIRECTION ( 'NONE',  ( 1.000000000000000000, 0.000000000000000000, 0.000000000000000000 ) ) ;
#12124 = CARTESIAN_POINT ( 'NONE',  ( 38.63098279924288647, -22.91368208888609814, 70.22690120949090442 ) ) ;
#12125 = EDGE_LOOP ( 'NONE', ( #18841, #20828, #24186, #5352 ) ) ;
#12126 = CARTESIAN_POINT ( 'NONE',  ( 40.31606138205700773, -20.57051414398581812, 75.95118011352499821 ) ) ;
#12127 = DIRECTION ( 'NONE',  ( 1.000000000000000000, 1.734723475976804876E-16, -1.734723475976814737E-16 ) ) ;
#12128 = ORIENTED_EDGE ( 'NONE', *, *, #19966, .T. ) ;
#12129 = ORIENTED_EDGE ( 'NONE', *, *, #13692, .F. ) ;
#12130 = PRODUCT_DEFINITION_CONTEXT ( 'detailed design', #6515, 'design' ) ;
#12131 = CARTESIAN_POINT ( 'NONE',  ( 38.37017380507018771, -25.60384086642191548, 69.04448340153878405 ) ) ;
#12132 = ADVANCED_FACE ( 'NONE', ( #6493 ), #419, .F. ) ;
#12133 = EDGE_CURVE ( 'NONE', #7783, #4335, #11663, .T. ) ;
#12134 = CARTESIAN_POINT ( 'NONE',  ( 36.87297107704152666, -25.71368208888609885, 72.49904802271738902 ) ) ;
#12135 = DIRECTION ( 'NONE',  ( 0.000000000000000000, -0.3299742535180970049, 0.9439899321577400748 ) ) ;
#12136 = ORIENTED_EDGE ( 'NONE', *, *, #15538, .F. ) ;
#12137 = DIRECTION ( 'NONE',  ( -1.000000000000000000, 6.938893903907231533E-15, 6.505213034912821500E-16 ) ) ;
#12138 = VERTEX_POINT ( 'NONE', #11925 ) ;
#12139 = CARTESIAN_POINT ( 'NONE',  ( 40.10709070826256806, -6.251773263459675434, 82.75068920652414306 ) ) ;
#12140 = DIRECTION ( 'NONE',  ( 1.000000000000000000, 0.000000000000000000, 0.000000000000000000 ) ) ;
#12141 = ADVANCED_FACE ( 'NONE', ( #13845 ), #22203, .F. ) ;
#12142 = CARTESIAN_POINT ( 'NONE',  ( 39.02088643472237806, -0.7038408664219175659, 73.73360434286902887 ) ) ;
#12143 = AXIS2_PLACEMENT_3D ( 'NONE', #8924, #17162, #16768 ) ;
#12144 = CARTESIAN_POINT ( 'NONE',  ( 33.31606138205700773, -0.3976309214372003575, 10.62865949386124242 ) ) ;
#12145 = CARTESIAN_POINT ( 'NONE',  ( 32.56606138205700773, 47.04446929126254417, 81.37823623207319201 ) ) ;
#12146 = CARTESIAN_POINT ( 'NONE',  ( 37.25202387243752611, -7.213682088886102406, 70.00779233799264034 ) ) ;
#12147 = DIRECTION ( 'NONE',  ( 0.000000000000000000, -0.6568589528324746407, 0.7540134720837717852 ) ) ;
#12148 = CARTESIAN_POINT ( 'NONE',  ( 39.98359781491296161, -24.41368208888610525, 71.86517103874045631 ) ) ;
#12149 = CIRCLE ( 'NONE', #13376, 3.999999999999997335 ) ;
#12150 = DIRECTION ( 'NONE',  ( 1.000000000000000000, 5.723954245484026287E-31, -8.237414899530862620E-31 ) ) ;
#12151 = ADVANCED_FACE ( 'NONE', ( #16144 ), #2239, .F. ) ;
#12152 = CARTESIAN_POINT ( 'NONE',  ( 39.98359781491296161, 0.7961591335780872081, 70.89533451361948835 ) ) ;
#12153 = CARTESIAN_POINT ( 'NONE',  ( 43.81608638205700146, -3.566646240838321269, 18.16837712155798457 ) ) ;
#12154 = CARTESIAN_POINT ( 'NONE',  ( 38.26194895904384197, -26.60384086642191193, 72.51602215082114355 ) ) ;
#12155 = CARTESIAN_POINT ( 'NONE',  ( 40.14115730948191185, -10.51368208888609956, 71.32335560751961623 ) ) ;
#12156 = PLANE ( 'NONE',  #13975 ) ;
#12157 = VECTOR ( 'NONE', #22280, 1000.000000000000000 ) ;
#12158 = CARTESIAN_POINT ( 'NONE',  ( 36.49096545463212493, -12.10384086642191193, 71.32335560751961623 ) ) ;
#12159 = CYLINDRICAL_SURFACE ( 'NONE', #8110, 1.000000000000000888 ) ;
#12160 = CARTESIAN_POINT ( 'NONE',  ( 37.69796330110504101, -9.113682088886100985, 69.66206559358663242 ) ) ;
#12161 = ORIENTED_EDGE ( 'NONE', *, *, #3486, .T. ) ;
#12162 = CARTESIAN_POINT ( 'NONE',  ( 36.36258059203031934, -15.71368208888610773, 72.86986841596736042 ) ) ;
#12163 = EDGE_LOOP ( 'NONE', ( #21626, #19910, #2626, #14495 ) ) ;
#12164 = CARTESIAN_POINT ( 'NONE',  ( 33.81606138205700063, 22.19123852234699967, 69.30501292736994401 ) ) ;
#12165 = DIRECTION ( 'NONE',  ( -1.000000000000000000, 0.000000000000000000, 0.000000000000000000 ) ) ;
#12166 = CARTESIAN_POINT ( 'NONE',  ( 39.31564783533279694, -17.30384086642191477, 70.72433947564853440 ) ) ;
#12167 = ORIENTED_EDGE ( 'NONE', *, *, #799, .F. ) ;
#12168 = ORIENTED_EDGE ( 'NONE', *, *, #15206, .F. ) ;
#12169 = DIRECTION ( 'NONE',  ( 0.000000000000000000, 0.6595716529892419189, -0.7516416929448759277 ) ) ;
#12170 = DIRECTION ( 'NONE',  ( 1.000000000000000000, 0.000000000000000000, 0.000000000000000000 ) ) ;
#12171 = CARTESIAN_POINT ( 'NONE',  ( 36.98690846071097127, -23.80384086642191477, 69.45876917294174291 ) ) ;
#12172 = CYLINDRICAL_SURFACE ( 'NONE', #9263, 0.5000000000000004441 ) ;
#12173 = CARTESIAN_POINT ( 'NONE',  ( 39.73277004305198545, 1.786317911113892043, 73.23812341099230139 ) ) ;
#12174 = DIRECTION ( 'NONE',  ( 0.000000000000000000, 0.7071067811865427988, 0.7071067811865521247 ) ) ;
#12175 = VECTOR ( 'NONE', #1897, 1000.000000000000000 ) ;
#12176 = EDGE_CURVE ( 'NONE', #16232, #11095, #16272, .T. ) ;
#12177 = VERTEX_POINT ( 'NONE', #4051 ) ;
#12178 = EDGE_CURVE ( 'NONE', #3043, #16154, #21953, .T. ) ;
#12179 = DIRECTION ( 'NONE',  ( 0.000000000000000000, -3.289120579329467819E-15, -1.000000000000000000 ) ) ;
#12180 = DIRECTION ( 'NONE',  ( -1.000000000000000000, 0.000000000000000000, 0.000000000000000000 ) ) ;
#12181 = CARTESIAN_POINT ( 'NONE',  ( 39.95015449827720744, -23.00384086642191050, 71.96809898377887293 ) ) ;
#12182 = CARTESIAN_POINT ( 'NONE',  ( 31.81606138205700418, 38.19123852234598360, 71.05501292736988717 ) ) ;
#12183 = ORIENTED_EDGE ( 'NONE', *, *, #7346, .F. ) ;
#12184 = DIRECTION ( 'NONE',  ( 0.000000000000000000, -2.999999999999999839E-15, -1.000000000000000000 ) ) ;
#12185 = CARTESIAN_POINT ( 'NONE',  ( 40.31606138205699352, -9.092667827980694284, 28.75914562266559926 ) ) ;
#12186 = CARTESIAN_POINT ( 'NONE',  ( 37.89291511884479036, -2.503840866421910505, 72.49843995877331793 ) ) ;
#12187 = LINE ( 'NONE', #20156, #4413 ) ;
#12188 = VERTEX_POINT ( 'NONE', #21825 ) ;
#12189 = EDGE_CURVE ( 'NONE', #16878, #8257, #6113, .T. ) ;
#12190 = CARTESIAN_POINT ( 'NONE',  ( 38.93415946300897446, -28.11368208888610098, 73.09843995877328382 ) ) ;
#12191 = ORIENTED_EDGE ( 'NONE', *, *, #9180, .T. ) ;
#12192 = VERTEX_POINT ( 'NONE', #6374 ) ;
#12193 = CARTESIAN_POINT ( 'NONE',  ( 46.81606138205707168, -37.26069504592553017, 64.48189387429259511 ) ) ;
#12194 = CYLINDRICAL_SURFACE ( 'NONE', #16619, 1.000000000000000888 ) ;
#12195 = CARTESIAN_POINT ( 'NONE',  ( 39.24876120206128860, -8.713682088886100630, 70.63227792289247020 ) ) ;
#12196 = CARTESIAN_POINT ( 'NONE',  ( 38.37017380507020192, -2.013682088886102228, 72.51602215082118619 ) ) ;
#12197 = EDGE_LOOP ( 'NONE', ( #19024, #11173, #23077, #21873 ) ) ;
#12198 = VERTEX_POINT ( 'NONE', #16018 ) ;
#12199 = LINE ( 'NONE', #12454, #9108 ) ;
#12200 = DIRECTION ( 'NONE',  ( 1.000000000000000000, 1.734723475976814737E-16, -1.734723475976809806E-16 ) ) ;
#12201 = DIRECTION ( 'NONE',  ( 0.000000000000000000, -2.999999999999999839E-15, -1.000000000000000000 ) ) ;
#12202 = CARTESIAN_POINT ( 'NONE',  ( 36.49096545463212493, -14.10384086642191015, 71.32335560751961623 ) ) ;
#12203 = CARTESIAN_POINT ( 'NONE',  ( 30.81606138205697931, -4.589472609077253296, -6.350807634294811876 ) ) ;
#12204 = LINE ( 'NONE', #14129, #4002 ) ;
#12205 = ORIENTED_EDGE ( 'NONE', *, *, #14928, .F. ) ;
#12206 = ORIENTED_EDGE ( 'NONE', *, *, #12651, .F. ) ;
#12207 = ORIENTED_EDGE ( 'NONE', *, *, #13592, .T. ) ;
#12208 = DIRECTION ( 'NONE',  ( 1.000000000000000000, 0.000000000000000000, 0.000000000000000000 ) ) ;
#12209 = CARTESIAN_POINT ( 'NONE',  ( 40.14115730948191185, -4.513682088886104005, 71.32335560751961623 ) ) ;
#12210 = CARTESIAN_POINT ( 'NONE',  ( 40.64099152588523367, 1.392818861812999964, 93.30501292736998664 ) ) ;
#12211 = PLANE ( 'NONE',  #10401 ) ;
#12212 = LINE ( 'NONE', #11967, #20954 ) ;
#12213 = CARTESIAN_POINT ( 'NONE',  ( 40.12624830571841983, -29.10876147765395672, 71.35553700530282129 ) ) ;
#12214 = PRODUCT_DEFINITION_SHAPE ( 'NONE', 'NONE',  #25495 ) ;
#12215 = FACE_OUTER_BOUND ( 'NONE', #6486, .T. ) ;
#12216 = LINE ( 'NONE', #10150, #6081 ) ;
#12217 = EDGE_CURVE ( 'NONE', #24906, #21235, #17849, .T. ) ;
#12218 = PLANE ( 'NONE',  #4556 ) ;
#12219 = ORIENTED_EDGE ( 'NONE', *, *, #18983, .T. ) ;
#12220 = VERTEX_POINT ( 'NONE', #5992 ) ;
#12221 = DIRECTION ( 'NONE',  ( 0.000000000000000000, 1.000000000000000000, -3.304235192336775512E-15 ) ) ;
#12222 = CARTESIAN_POINT ( 'NONE',  ( 36.36258059203030513, -5.903840866421909972, 69.89063713639259845 ) ) ;
#12223 = EDGE_LOOP ( 'NONE', ( #21441, #18254, #15758, #18829 ) ) ;
#12224 = DIRECTION ( 'NONE',  ( 0.000000000000000000, 2.999999999999999839E-15, 1.000000000000000000 ) ) ;
#12225 = CARTESIAN_POINT ( 'NONE',  ( 36.68196826583682935, -5.613682088886105426, 71.96809898377890136 ) ) ;
#12226 = CARTESIAN_POINT ( 'NONE',  ( 38.31606138205695089, 2.967040633637578750, 4.322985289651505525 ) ) ;
#12227 = CARTESIAN_POINT ( 'NONE',  ( 36.29569395875879678, -17.31368208888610383, 69.98269868914867686 ) ) ;
#12228 = EDGE_CURVE ( 'NONE', #15455, #17954, #15895, .T. ) ;
#12229 = CARTESIAN_POINT ( 'NONE',  ( 43.14003743237937982, 2.901513403460370455, 6.097021259270054117 ) ) ;
#12230 = DIRECTION ( 'NONE',  ( 0.000000000000000000, -0.5706330172266919076, 0.8212051873014208914 ) ) ;
#12231 = ADVANCED_FACE ( 'NONE', ( #23751 ), #10235, .F. ) ;
#12232 = CIRCLE ( 'NONE', #1099, 10.49999999999999822 ) ;
#12233 = FACE_OUTER_BOUND ( 'NONE', #24245, .T. ) ;
#12234 = EDGE_CURVE ( 'NONE', #22820, #3395, #4439, .T. ) ;
#12235 = SURFACE_SIDE_STYLE ('',( #16082 ) ) ;
#12236 = AXIS2_PLACEMENT_3D ( 'NONE', #5728, #11541, #9613 ) ;
#12237 = VECTOR ( 'NONE', #17308, 1000.000000000000000 ) ;
#12238 = DIRECTION ( 'NONE',  ( -1.000000000000000000, -3.091505625455828697E-15, -4.515976121274771690E-17 ) ) ;
#12239 = CARTESIAN_POINT ( 'NONE',  ( 44.81606138205700063, -26.74044063519535186, 82.55501292737007191 ) ) ;
#12240 = LINE ( 'NONE', #15955, #6551 ) ;
#12241 = CARTESIAN_POINT ( 'NONE',  ( 39.31564783533280405, -26.31368208888610027, 72.03616607671136762 ) ) ;
#12242 = EDGE_LOOP ( 'NONE', ( #5562, #2502, #10521, #19400, #22180, #4185, #7778, #16065 ) ) ;
#12243 = CARTESIAN_POINT ( 'NONE',  ( 39.53940869104339839, -21.82950711158638768, 75.81284195793978142 ) ) ;
#12244 = EDGE_CURVE ( 'NONE', #22626, #20166, #11255, .T. ) ;
#12245 = DIRECTION ( 'NONE',  ( 0.000000000000000000, -0.6568589528324746407, 0.7540134720837717852 ) ) ;
#12246 = ORIENTED_EDGE ( 'NONE', *, *, #994, .T. ) ;
#12247 = ORIENTED_EDGE ( 'NONE', *, *, #17948, .T. ) ;
#12248 = CARTESIAN_POINT ( 'NONE',  ( 39.12911128074872380, -23.50384086642191050, 69.06206559358665231 ) ) ;
#12249 = CARTESIAN_POINT ( 'NONE',  ( 40.52078840805428683, 1.386317911113894130, 70.60699637195612866 ) ) ;
#12250 = CARTESIAN_POINT ( 'NONE',  ( 29.81606138205707879, -38.42645682328038959, 63.90656833300437256 ) ) ;
#12251 = AXIS2_PLACEMENT_3D ( 'NONE', #14966, #5185, #13039 ) ;
#12252 = CIRCLE ( 'NONE', #6891, 1.750000000000001554 ) ;
#12253 = CIRCLE ( 'NONE', #7726, 0.4999999999999994449 ) ;
#12254 = FACE_OUTER_BOUND ( 'NONE', #15491, .T. ) ;
#12255 = ORIENTED_EDGE ( 'NONE', *, *, #21384, .F. ) ;
#12256 = CARTESIAN_POINT ( 'NONE',  ( 39.18866295275135769, -5.390573154769174202, 82.80338437050654932 ) ) ;
#12257 = CARTESIAN_POINT ( 'NONE',  ( 36.31606138205700063, 41.44123852234599781, 75.30501292736987295 ) ) ;
#12258 = CARTESIAN_POINT ( 'NONE',  ( 40.33642880535521869, -5.303840866421911215, 69.98269868914867686 ) ) ;
#12259 = ADVANCED_FACE ( 'NONE', ( #17972 ), #12053, .F. ) ;
#12260 = CARTESIAN_POINT ( 'NONE',  ( 30.81606138205707879, -39.99575152356569419, 63.13209164280871022 ) ) ;
#12261 = FACE_BOUND ( 'NONE', #23951, .T. ) ;
#12262 = CARTESIAN_POINT ( 'NONE',  ( 37.69796330110504101, -9.113682088886100985, 69.66206559358663242 ) ) ;
#12263 = CARTESIAN_POINT ( 'NONE',  ( 43.81606138205700063, 4.103895195095678794, 6.341006091748962348 ) ) ;
#12264 = ADVANCED_FACE ( 'NONE', ( #24116 ), #10357, .T. ) ;
#12265 = DIRECTION ( 'NONE',  ( -1.000000000000000000, -7.497642437004238434E-16, 3.111695294957277996E-17 ) ) ;
#12266 = EDGE_CURVE ( 'NONE', #17894, #19306, #21942, .T. ) ;
#12267 = EDGE_CURVE ( 'NONE', #11848, #9810, #23633, .T. ) ;
#12268 = ADVANCED_FACE ( 'NONE', ( #18349 ), #24372, .F. ) ;
#12269 = LINE ( 'NONE', #4279, #20062 ) ;
#12270 = DIRECTION ( 'NONE',  ( 0.000000000000000000, -0.5706330172266915746, 0.8212051873014213355 ) ) ;
#12271 = AXIS2_PLACEMENT_3D ( 'NONE', #19808, #14015, #2144 ) ;
#12272 = CARTESIAN_POINT ( 'NONE',  ( 43.31606138205700063, -12.40281258615395465, 20.95421293576468358 ) ) ;
#12273 =( BOUNDED_CURVE ( )  B_SPLINE_CURVE ( 3, ( #9365, #17214, #25035, #8334 ),
 .UNSPECIFIED., .F., .T. ) 
 B_SPLINE_CURVE_WITH_KNOTS ( ( 4, 4 ),
 ( 0.000000000000000000, 1.570796326794895004 ),
 .UNSPECIFIED. ) 
 CURVE ( )  GEOMETRIC_REPRESENTATION_ITEM ( )  RATIONAL_B_SPLINE_CURVE ( ( 1.000000000000000000, 0.8047378541243649375, 0.8047378541243649375, 1.000000000000000000 ) ) 
 REPRESENTATION_ITEM ( '' )  );
#12274 = CARTESIAN_POINT ( 'NONE',  ( 39.02742774030101458, -27.40384086642191619, 70.49320253461758057 ) ) ;
#12275 = CARTESIAN_POINT ( 'NONE',  ( 37.25202387243752611, -13.21368208888610063, 70.00779233799262613 ) ) ;
#12276 = DIRECTION ( 'NONE',  ( -1.000000000000000000, 0.000000000000000000, 0.000000000000000000 ) ) ;
#12277 = ADVANCED_FACE ( 'NONE', ( #4805 ), #2992, .T. ) ;
#12278 = CARTESIAN_POINT ( 'NONE',  ( 36.64852494920107517, -14.20384086642191157, 71.86517103874048473 ) ) ;
#12279 = CARTESIAN_POINT ( 'NONE',  ( 30.81606138205697931, -4.589472609077253296, -6.350807634294811876 ) ) ;
#12280 =( REPRESENTATION_RELATIONSHIP ('NONE','NONE', #17377, #24379 ) REPRESENTATION_RELATIONSHIP_WITH_TRANSFORMATION ( #13560 )SHAPE_REPRESENTATION_RELATIONSHIP( ) );
#12281 = CARTESIAN_POINT ( 'NONE',  ( 36.80608444377001121, -11.31368208888609672, 70.35351908239857721 ) ) ;
#12282 = EDGE_LOOP ( 'NONE', ( #20827, #13820, #12679, #19760 ) ) ;
#12283 = CARTESIAN_POINT ( 'NONE',  ( 39.12911128074873801, -14.11368208888610987, 73.69843995877327814 ) ) ;
#12284 = ORIENTED_EDGE ( 'NONE', *, *, #10523, .F. ) ;
#12285 = DIRECTION ( 'NONE',  ( -1.000000000000000000, -2.999999999999999839E-15, 0.000000000000000000 ) ) ;
#12286 = DIRECTION ( 'NONE',  ( 0.000000000000000000, 0.1918498038142812112, -0.9814242980364923374 ) ) ;
#12287 = CARTESIAN_POINT ( 'NONE',  ( 37.31647492878124694, -18.30384086642191122, 72.03616607671141026 ) ) ;
#12288 = ORIENTED_EDGE ( 'NONE', *, *, #20302, .T. ) ;
#12289 = EDGE_CURVE ( 'NONE', #4665, #2525, #540, .T. ) ;
#12290 = ORIENTED_EDGE ( 'NONE', *, *, #19252, .F. ) ;
#12291 = CYLINDRICAL_SURFACE ( 'NONE', #1807, 2.000000000000000000 ) ;
#12292 = CARTESIAN_POINT ( 'NONE',  ( 30.81606138205700418, 0.3928188618129990761, 82.55501292736998664 ) ) ;
#12293 = CARTESIAN_POINT ( 'NONE',  ( 35.86008812008917346, -22.10384086642191548, 71.32335560751961623 ) ) ;
#12294 = VECTOR ( 'NONE', #4220, 1000.000000000000000 ) ;
#12295 = DIRECTION ( 'NONE',  ( 0.000000000000000000, 0.4425581086832394706, -0.8967398287344628960 ) ) ;
#12296 = CARTESIAN_POINT ( 'NONE',  ( 39.29254315202756231, -28.81368208888610383, 69.94417936956671156 ) ) ;
#12297 = CARTESIAN_POINT ( 'NONE',  ( 36.31606138205700063, -4.357181138186123626, 83.30501292736992980 ) ) ;
#12298 = VERTEX_POINT ( 'NONE', #6748 ) ;
#12299 = PRESENTATION_LAYER_ASSIGNMENT (  '', '', ( #9829 ) ) ;
#12300 = VERTEX_POINT ( 'NONE', #16662 ) ;
#12301 = CARTESIAN_POINT ( 'NONE',  ( 33.80700582398836218, 3.227014992217502876, 6.369498915812659590 ) ) ;
#12302 = DIRECTION ( 'NONE',  ( 0.000000000000000000, 1.000000000000000000, -2.921639538487253867E-15 ) ) ;
#12303 = CARTESIAN_POINT ( 'NONE',  ( 36.80608444377002542, -14.30384086642191299, 72.40698646996133903 ) ) ;
#12304 = SURFACE_STYLE_FILL_AREA ( #19899 ) ;
#12305 = DIRECTION ( 'NONE',  ( 1.000000000000000000, 2.973811673103095397E-15, 0.000000000000000000 ) ) ;
#12306 =( GEOMETRIC_REPRESENTATION_CONTEXT ( 3 ) GLOBAL_UNCERTAINTY_ASSIGNED_CONTEXT ( ( #19780 ) ) GLOBAL_UNIT_ASSIGNED_CONTEXT ( ( #6888, #693, #3012 ) ) REPRESENTATION_CONTEXT ( 'NONE', 'WORKASPACE' ) );
#12307 = CARTESIAN_POINT ( 'NONE',  ( 40.31606138205700773, -31.05876147765399864, 74.30501292737010033 ) ) ;
#12308 = DIRECTION ( 'NONE',  ( 0.000000000000000000, -2.999999999999999839E-15, -1.000000000000000000 ) ) ;
#12309 = CARTESIAN_POINT ( 'NONE',  ( 37.38336156205273397, 0.09615913357808798800, 70.63227792289248441 ) ) ;
#12310 = LINE ( 'NONE', #8439, #24142 ) ;
#12311 = ORIENTED_EDGE ( 'NONE', *, *, #22807, .F. ) ;
#12312 = VECTOR ( 'NONE', #24373, 1000.000000000000114 ) ;
#12313 = CARTESIAN_POINT ( 'NONE',  ( 40.14115730948191185, -28.51368208888610667, 71.32335560751958781 ) ) ;
#12314 = ORIENTED_EDGE ( 'NONE', *, *, #3445, .T. ) ;
#12315 = ORIENTED_EDGE ( 'NONE', *, *, #15530, .F. ) ;
#12316 = CARTESIAN_POINT ( 'NONE',  ( 33.66606138205698073, -5.898435835062239008, -2.003809078978638247 ) ) ;
#12318 = ADVANCED_FACE ( 'NONE', ( #12686 ), #9078, .T. ) ;
#12317 = DIRECTION ( 'NONE',  ( 0.000000000000000000, 0.000000000000000000, 1.000000000000000000 ) ) ;
#12319 = CARTESIAN_POINT ( 'NONE',  ( 37.31647492878122563, -5.313682088886097610, 70.72433947564853440 ) ) ;
#12320 = VECTOR ( 'NONE', #20210, 1000.000000000000000 ) ;
#12321 = ADVANCED_FACE ( 'NONE', ( #24753 ), #18727, .F. ) ;
#12322 = CARTESIAN_POINT ( 'NONE',  ( 39.24876120206128860, -2.713682088886101962, 70.63227792289247020 ) ) ;
#12323 = EDGE_LOOP ( 'NONE', ( #25025, #20469, #10370, #10480 ) ) ;
#12324 = PRODUCT_RELATED_PRODUCT_CATEGORY ( 'part', '', ( #19167 ) ) ;
#12325 = ORIENTED_EDGE ( 'NONE', *, *, #2054, .F. ) ;
#12326 = CARTESIAN_POINT ( 'NONE',  ( 45.81606138205700063, -30.95005513552129983, 81.04249030099066431 ) ) ;
#12327 = LINE ( 'NONE', #18247, #20272 ) ;
#12328 = ORIENTED_EDGE ( 'NONE', *, *, #20103, .T. ) ;
#12329 = CARTESIAN_POINT ( 'NONE',  ( 33.81606138205700063, 16.19123852234701388, 73.80501292736995822 ) ) ;
#12330 = CARTESIAN_POINT ( 'NONE',  ( 36.80608444377001831, -10.30384086642191654, 72.40698646996136745 ) ) ;
#12331 = VECTOR ( 'NONE', #20765, 1000.000000000000000 ) ;
#12332 = CARTESIAN_POINT ( 'NONE',  ( 43.81606138205700063, 38.19123852234599070, 73.05501292736988717 ) ) ;
#12333 = ORIENTED_EDGE ( 'NONE', *, *, #11768, .F. ) ;
#12334 = ORIENTED_EDGE ( 'NONE', *, *, #10556, .T. ) ;
#12335 = ORIENTED_EDGE ( 'NONE', *, *, #15930, .F. ) ;
#12336 = AXIS2_PLACEMENT_3D ( 'NONE', #19604, #10088, #14070 ) ;
#12337 = CARTESIAN_POINT ( 'NONE',  ( 43.05893433410182070, 3.408565912792066221, 6.350990188909392486 ) ) ;
#12338 = CARTESIAN_POINT ( 'NONE',  ( 36.64852494920107517, -9.413682088886107024, 70.89533451361948835 ) ) ;
#12339 = EDGE_CURVE ( 'NONE', #5120, #17340, #805, .T. ) ;
#12340 = CARTESIAN_POINT ( 'NONE',  ( 39.31606138205700063, 43.19123852234599070, 73.55501292736987295 ) ) ;
#12341 = CARTESIAN_POINT ( 'NONE',  ( 38.31606138205712853, 42.19123852234599781, 75.30501292736987295 ) ) ;
#12342 = VECTOR ( 'NONE', #1411, 1000.000000000000000 ) ;
#12343 = CARTESIAN_POINT ( 'NONE',  ( 36.64852494920107517, -23.41368208888610525, 70.89533451361945993 ) ) ;
#12344 = CARTESIAN_POINT ( 'NONE',  ( 40.20492003450708296, -29.10876147765143074, 70.86866654954431510 ) ) ;
#12345 = VECTOR ( 'NONE', #14883, 1000.000000000000000 ) ;
#12346 = DIRECTION ( 'NONE',  ( 1.000000000000000000, 0.000000000000000000, 0.000000000000000000 ) ) ;
#12347 = CARTESIAN_POINT ( 'NONE',  ( 44.06606138205700063, 45.04446929126260102, 82.37823623207320622 ) ) ;
#12348 = CIRCLE ( 'NONE', #22607, 1.000000000000000888 ) ;
#12349 = CARTESIAN_POINT ( 'NONE',  ( 31.81606138205700418, -24.55876147765400574, 72.80501292737008612 ) ) ;
#12350 = ORIENTED_EDGE ( 'NONE', *, *, #14939, .T. ) ;
#12351 = ORIENTED_EDGE ( 'NONE', *, *, #24955, .F. ) ;
#12353 = ADVANCED_FACE ( 'NONE', ( #16395 ), #6615, .T. ) ;
#12352 = CARTESIAN_POINT ( 'NONE',  ( 43.31606138205700773, -19.73594837544666802, 24.33996001444790025 ) ) ;
#12354 = CARTESIAN_POINT ( 'NONE',  ( 36.89935272106205133, -2.403840866421917521, 73.23812341099225875 ) ) ;
#12355 = VECTOR ( 'NONE', #15901, 1000.000000000000000 ) ;
#12356 = EDGE_CURVE ( 'NONE', #13535, #9362, #18592, .T. ) ;
#12357 = ORIENTED_EDGE ( 'NONE', *, *, #6812, .F. ) ;
#12358 = ORIENTED_EDGE ( 'NONE', *, *, #14230, .T. ) ;
#12359 = PLANE ( 'NONE',  #2947 ) ;
#12360 = CARTESIAN_POINT ( 'NONE',  ( 37.25202387243752611, -11.21368208888610241, 70.00779233799262613 ) ) ;
#12361 = AXIS2_PLACEMENT_3D ( 'NONE', #19121, #18861, #7400 ) ;
#12362 = FACE_OUTER_BOUND ( 'NONE', #6555, .T. ) ;
#12363 = CARTESIAN_POINT ( 'NONE',  ( 37.61123632939165873, -17.91368208888610525, 73.73360434286898624 ) ) ;
#12364 = AXIS2_PLACEMENT_3D ( 'NONE', #12509, #4630, #4505 ) ;
#12365 = DIRECTION ( 'NONE',  ( 0.000000000000000000, 0.5706330172266919076, -0.8212051873014208914 ) ) ;
#12366 = CARTESIAN_POINT ( 'NONE',  ( 45.81606138205697221, -4.349482454670838827, -5.142398479549302515 ) ) ;
#12367 = EDGE_CURVE ( 'NONE', #20521, #13577, #23570, .T. ) ;
#12368 = DIRECTION ( 'NONE',  ( 0.000000000000000000, 3.491481338843134933E-15, 1.000000000000000000 ) ) ;
#12369 =( NAMED_UNIT ( * ) PLANE_ANGLE_UNIT ( ) SI_UNIT ( $, .RADIAN. ) );
#12370 = FACE_OUTER_BOUND ( 'NONE', #15620, .T. ) ;
#12371 = PRODUCT_DEFINITION_SHAPE ( 'NONE', 'NONE',  #25498 ) ;
#12372 = DIRECTION ( 'NONE',  ( 0.000000000000000000, 0.6568589528324746407, -0.7540134720837717852 ) ) ;
#12373 = PLANE ( 'NONE',  #6139 ) ;
#12374 = CARTESIAN_POINT ( 'NONE',  ( 37.25260217561390874, -23.61368208888610098, 71.78268878715390144 ) ) ;
#12375 = EDGE_LOOP ( 'NONE', ( #8632, #5100, #24254, #1798 ) ) ;
#12376 = CARTESIAN_POINT ( 'NONE',  ( 40.26527270485448184, -20.81370745732132832, 75.90702589141309886 ) ) ;
#12377 = PLANE ( 'NONE',  #13601 ) ;
#12378 = ORIENTED_EDGE ( 'NONE', *, *, #23502, .T. ) ;
#12379 = EDGE_LOOP ( 'NONE', ( #17093, #324, #19153, #364 ) ) ;
#12380 = VECTOR ( 'NONE', #7711, 1000.000000000000114 ) ;
#12381 = CARTESIAN_POINT ( 'NONE',  ( 36.98690846071097127, -25.80384086642191477, 69.45876917294174291 ) ) ;
#12382 = CARTESIAN_POINT ( 'NONE',  ( 40.55423172469004811, 1.586317911113896306, 72.05058123536544201 ) ) ;
#12383 = CARTESIAN_POINT ( 'NONE',  ( 32.81606138205700773, 39.19123852234599070, 72.05501292736988717 ) ) ;
#12384 = FACE_OUTER_BOUND ( 'NONE', #11853, .T. ) ;
#12385 =( LENGTH_UNIT ( ) NAMED_UNIT ( * ) SI_UNIT ( .MILLI., .METRE. ) );
#12386 = ORIENTED_EDGE ( 'NONE', *, *, #1756, .T. ) ;
#12387 = CARTESIAN_POINT ( 'NONE',  ( 43.39709375099405975, 3.108381023609500193, 6.137326095127844994 ) ) ;
#12388 = CARTESIAN_POINT ( 'NONE',  ( 32.81606138205700773, 18.19123852234599070, 72.05501292736995822 ) ) ;
#12389 = CARTESIAN_POINT ( 'NONE',  ( 35.86008812008917346, -2.103840866421915923, 71.32335560751961623 ) ) ;
#12390 = CARTESIAN_POINT ( 'NONE',  ( 33.31606138205700773, 3.195231713396695650, 64.80689721350518084 ) ) ;
#12391 = DIRECTION ( 'NONE',  ( -0.000000000000000000, -0.9814242980364923374, -0.1918498038142812112 ) ) ;
#12392 = CARTESIAN_POINT ( 'NONE',  ( 36.87297107704152666, -9.713682088886107735, 72.49904802271743165 ) ) ;
#12393 = DIRECTION ( 'NONE',  ( 0.000000000000000000, 0.9992330079037401447, -0.03915859951076000600 ) ) ;
#12394 = VECTOR ( 'NONE', #14803, 1000.000000000000000 ) ;
#12395 = ADVANCED_FACE ( 'NONE', ( #5200 ), #20275, .T. ) ;
#12396 = CARTESIAN_POINT ( 'NONE',  ( 36.68196826583682935, -27.61368208888610809, 71.96809898377887293 ) ) ;
#12397 = AXIS2_PLACEMENT_3D ( 'NONE', #6001, #10245, #2247 ) ;
#12398 = LINE ( 'NONE', #22291, #7725 ) ;
#12399 = DIRECTION ( 'NONE',  ( 0.000000000000000000, 0.7540134720837717852, 0.6568589528324746407 ) ) ;
#12400 = CARTESIAN_POINT ( 'NONE',  ( 37.25260217561390874, -26.00384086642191406, 70.97781676520601479 ) ) ;
#12401 = CARTESIAN_POINT ( 'NONE',  ( 36.80608444377001121, -13.31368208888609672, 70.35351908239857721 ) ) ;
#12402 = DIRECTION ( 'NONE',  ( -1.000000000000000000, 0.000000000000000000, 0.000000000000000000 ) ) ;
#12403 = EDGE_LOOP ( 'NONE', ( #5421, #9317, #13949, #6313 ) ) ;
#12404 = CARTESIAN_POINT ( 'NONE',  ( 39.38009889167648936, -9.403840866421907307, 70.00779233799264034 ) ) ;
#12405 = EDGE_CURVE ( 'NONE', #3835, #19999, #2599, .T. ) ;
#12406 = DIRECTION ( 'NONE',  ( 1.000000000000000000, 1.734723475976804876E-16, -1.734723475976814737E-16 ) ) ;
#12407 = EDGE_CURVE ( 'NONE', #17256, #3766, #788, .T. ) ;
#12408 = CARTESIAN_POINT ( 'NONE',  ( 38.26194895904383486, -5.013682088886102228, 69.64448340153879258 ) ) ;
#12409 = ORIENTED_EDGE ( 'NONE', *, *, #19958, .T. ) ;
#12410 = CARTESIAN_POINT ( 'NONE',  ( 39.73277004305198545, -18.21368208888610596, 73.23812341099225875 ) ) ;
#12411 = EDGE_LOOP ( 'NONE', ( #8282, #13107, #18721, #22929 ) ) ;
#12412 = DIRECTION ( 'NONE',  ( 0.000000000000000000, -0.3299742535180969494, 0.9439899321577399638 ) ) ;
#12413 = EDGE_CURVE ( 'NONE', #8243, #11199, #22709, .T. ) ;
#12414 = DIRECTION ( 'NONE',  ( -1.000000000000000000, 0.000000000000000000, 0.000000000000000000 ) ) ;
#12415 = AXIS2_PLACEMENT_3D ( 'NONE', #16806, #8961, #14370 ) ;
#12416 = CARTESIAN_POINT ( 'NONE',  ( 38.00113996487112189, -15.70384086642191157, 70.22690120949090442 ) ) ;
#12417 = EDGE_CURVE ( 'NONE', #25304, #3155, #22583, .T. ) ;
#12418 = EDGE_CURVE ( 'NONE', #2564, #3312, #10995, .T. ) ;
#12419 = ORIENTED_EDGE ( 'NONE', *, *, #9650, .F. ) ;
#12420 = ORIENTED_EDGE ( 'NONE', *, *, #5079, .F. ) ;
#12421 = CARTESIAN_POINT ( 'NONE',  ( 43.06606138205700063, 42.19123852234601202, 79.18605660143489899 ) ) ;
#12422 = CARTESIAN_POINT ( 'NONE',  ( 34.81606138205687273, 42.19123852234595518, 61.30501292736988006 ) ) ;
#12423 = CARTESIAN_POINT ( 'NONE',  ( 37.61123632939164452, -21.70384086642190979, 69.02690120949091579 ) ) ;
#12424 = CARTESIAN_POINT ( 'NONE',  ( 43.31606138205700063, -20.88462213365835041, 44.49284693532412405 ) ) ;
#12425 = CARTESIAN_POINT ( 'NONE',  ( 39.64521430340304420, 1.186317911113898838, 69.45876917294178554 ) ) ;
#12426 = DIRECTION ( 'NONE',  ( 0.000000000000000000, -0.6568589528324746407, 0.7540134720837716742 ) ) ;
#12427 = EDGE_CURVE ( 'NONE', #24509, #23758, #20791, .T. ) ;
#12428 = DIRECTION ( 'NONE',  ( 0.000000000000000000, -0.4278636397681519488, 0.9038432971286277651 ) ) ;
#12429 = EDGE_CURVE ( 'NONE', #9362, #2551, #3383, .T. ) ;
#12430 = VERTEX_POINT ( 'NONE', #1819 ) ;
#12431 = ORIENTED_EDGE ( 'NONE', *, *, #12633, .F. ) ;
#12432 = CARTESIAN_POINT ( 'NONE',  ( 29.81606138205707168, -36.80651332587436286, 65.82119181171029254 ) ) ;
#12433 = DIRECTION ( 'NONE',  ( -1.000000000000000000, -1.734723475976804876E-16, 1.734723475976814737E-16 ) ) ;
#12434 = CARTESIAN_POINT ( 'NONE',  ( 37.80618814713138676, -11.70384086642190802, 69.62690120949091011 ) ) ;
#12435 =( LENGTH_UNIT ( ) NAMED_UNIT ( * ) SI_UNIT ( .MILLI., .METRE. ) );
#12436 = VECTOR ( 'NONE', #22383, 1000.000000000000000 ) ;
#12437 = DIRECTION ( 'NONE',  ( -1.000000000000000000, 0.000000000000000000, 0.000000000000000000 ) ) ;
#12438 = LINE ( 'NONE', #16273, #12312 ) ;
#12439 = EDGE_CURVE ( 'NONE', #5442, #16465, #17556, .T. ) ;
#12440 = VECTOR ( 'NONE', #14973, 1000.000000000000000 ) ;
#12441 = CARTESIAN_POINT ( 'NONE',  ( 33.31606138205700773, -5.204193249396277032, 83.30501292736992980 ) ) ;
#12442 = CARTESIAN_POINT ( 'NONE',  ( 39.98359781491296161, -29.20384086642191335, 70.89533451361944572 ) ) ;
#12443 = DIRECTION ( 'NONE',  ( 4.542565983319590233E-31, 1.000000000000000000, -2.999999999999999839E-15 ) ) ;
#12444 = ORIENTED_EDGE ( 'NONE', *, *, #14126, .T. ) ;
#12445 = CARTESIAN_POINT ( 'NONE',  ( 39.82603832034400426, -28.31368208888610027, 72.40698646996131060 ) ) ;
#12446 = ORIENTED_EDGE ( 'NONE', *, *, #16170, .F. ) ;
#12447 = ORIENTED_EDGE ( 'NONE', *, *, #5771, .F. ) ;
#12448 = DIRECTION ( 'NONE',  ( -1.327674326049719602E-15, 0.4425581086832399147, -0.8967398287344627850 ) ) ;
#12449 = DIRECTION ( 'NONE',  ( 0.000000000000000000, 1.000000000000000000, -2.643388153869420409E-15 ) ) ;
#12450 = CARTESIAN_POINT ( 'NONE',  ( 37.60469502381300089, -5.213682088886100630, 70.49320253461759478 ) ) ;
#12451 = CARTESIAN_POINT ( 'NONE',  ( 37.12184278917507640, -1.513682088886101784, 71.43714994484035685 ) ) ;
#12452 = ORIENTED_EDGE ( 'NONE', *, *, #11505, .T. ) ;
#12453 = EDGE_LOOP ( 'NONE', ( #11227, #12480, #19812, #25049, #16286, #12284, #2493, #11815 ) ) ;
#12454 = CARTESIAN_POINT ( 'NONE',  ( 43.81606138205700063, 41.44123852234597649, 68.80501292736988717 ) ) ;
#12455 = CARTESIAN_POINT ( 'NONE',  ( 41.81606138205696510, -0.8482369431493732570, -3.067843137301039302 ) ) ;
#12456 = EDGE_LOOP ( 'NONE', ( #3338, #18464, #16098, #15751 ) ) ;
#12457 = FILL_AREA_STYLE ('',( #1078 ) ) ;
#12458 = VECTOR ( 'NONE', #7439, 1000.000000000000000 ) ;
#12459 = CARTESIAN_POINT ( 'NONE',  ( 39.38009889167648936, -9.403840866421907307, 70.00779233799264034 ) ) ;
#12460 = CIRCLE ( 'NONE', #5038, 1.750000000000000222 ) ;
#12461 = DIRECTION ( 'NONE',  ( -1.000000000000000000, -3.046345864243081103E-15, -1.366653866685768465E-16 ) ) ;
#12462 = CIRCLE ( 'NONE', #8333, 0.4999999999999998890 ) ;
#12463 = DIRECTION ( 'NONE',  ( -0.1733269559585477460, -5.551115123125804790E-15, -0.9848643390529193686 ) ) ;
#12464 = ORIENTED_EDGE ( 'NONE', *, *, #17948, .F. ) ;
#12465 = ORIENTED_EDGE ( 'NONE', *, *, #6948, .T. ) ;
#12466 = VERTEX_POINT ( 'NONE', #19476 ) ;
#12467 = DIRECTION ( 'NONE',  ( 1.734723475976805122E-16, -1.000000000000000000, 0.000000000000000000 ) ) ;
#12468 = CARTESIAN_POINT ( 'NONE',  ( 38.37017380507020192, -10.01368208888611022, 73.11602215082118050 ) ) ;
#12469 = AXIS2_PLACEMENT_3D ( 'NONE', #7606, #25085, #15449 ) ;
#12470 = CARTESIAN_POINT ( 'NONE',  ( 39.72979056325730340, -29.10876147765396738, 70.86673335466467449 ) ) ;
#12471 = DIRECTION ( 'NONE',  ( 0.000000000000000000, 0.6568589528324746407, -0.7540134720837717852 ) ) ;
#12472 = CARTESIAN_POINT ( 'NONE',  ( 36.81606138205700063, -1.054793099133682244, 61.76760556592023477 ) ) ;
#12473 = EDGE_CURVE ( 'NONE', #24159, #24513, #25258, .T. ) ;
#12474 = EDGE_CURVE ( 'NONE', #10887, #24226, #4654, .T. ) ;
#12475 = VECTOR ( 'NONE', #17467, 1000.000000000000000 ) ;
#12476 = CARTESIAN_POINT ( 'NONE',  ( 40.81606138205700773, -6.959910619544160681, 20.07251914782758107 ) ) ;
#12477 = DIRECTION ( 'NONE',  ( -1.734723475976804876E-16, -3.491481338843135327E-15, -1.000000000000000000 ) ) ;
#12478 = VECTOR ( 'NONE', #6512, 1000.000000000000000 ) ;
#12479 = DIRECTION ( 'NONE',  ( -1.000000000000000000, -1.445602896647339903E-16, 4.336808689942019400E-31 ) ) ;
#12480 = ORIENTED_EDGE ( 'NONE', *, *, #8021, .F. ) ;
#12481 = ORIENTED_EDGE ( 'NONE', *, *, #21218, .F. ) ;
#12482 = DIRECTION ( 'NONE',  ( 0.000000000000000000, 0.9814242980364923374, 0.1918498038142812112 ) ) ;
#12483 = CARTESIAN_POINT ( 'NONE',  ( 39.64521430340304420, -28.81368208888610383, 69.45876917294174291 ) ) ;
#12484 = CARTESIAN_POINT ( 'NONE',  ( 39.37952058850012804, -26.61368208888610809, 70.97781676520600058 ) ) ;
#12485 = ORIENTED_EDGE ( 'NONE', *, *, #15855, .F. ) ;
#12486 = AXIS2_PLACEMENT_3D ( 'NONE', #961, #24522, #4968 ) ;
#12487 = ORIENTED_EDGE ( 'NONE', *, *, #13372, .T. ) ;
#12488 = DIRECTION ( 'NONE',  ( 1.000000000000000000, 0.000000000000000000, 0.000000000000000000 ) ) ;
#12489 = CARTESIAN_POINT ( 'NONE',  ( 39.38009889167650357, -10.21368208888610773, 72.75271321436733274 ) ) ;
#12490 = CARTESIAN_POINT ( 'NONE',  ( 37.21915885897815457, -2.203840866421911571, 71.67976084211552745 ) ) ;
#12491 = CARTESIAN_POINT ( 'NONE',  ( 36.81606138205700063, -3.742417511052531509, 58.76316301854844681 ) ) ;
#12492 = VECTOR ( 'NONE', #11781, 1000.000000000000000 ) ;
#12493 = CARTESIAN_POINT ( 'NONE',  ( 38.26194895904383486, -7.013682088886100452, 69.04448340153881247 ) ) ;
#12494 = AXIS2_PLACEMENT_3D ( 'NONE', #262, #4902, #16360 ) ;
#12495 = DIRECTION ( 'NONE',  ( 1.000000000000000000, 0.000000000000000000, 0.000000000000000000 ) ) ;
#12496 = CARTESIAN_POINT ( 'NONE',  ( 31.81606138205700418, -36.30035594811090505, 74.91924054225879104 ) ) ;
#12497 = VECTOR ( 'NONE', #661, 1000.000000000000000 ) ;
#12498 = CARTESIAN_POINT ( 'NONE',  ( 33.91911362184673351, 2.753402311566605309, 6.093967742448072933 ) ) ;
#12499 = ADVANCED_FACE ( 'NONE', ( #21168 ), #9705, .F. ) ;
#12500 = CARTESIAN_POINT ( 'NONE',  ( 43.26087622013976386, 3.761531814868369406, 6.334937692063231651 ) ) ;
#12501 = EDGE_CURVE ( 'NONE', #6757, #17565, #9219, .T. ) ;
#12502 = CARTESIAN_POINT ( 'NONE',  ( 40.31606138205700773, -7.108002773205779334, 82.61702262452435264 ) ) ;
#12503 = VECTOR ( 'NONE', #6995, 1000.000000000000000 ) ;
#12504 = ADVANCED_FACE ( 'NONE', ( #11128 ), #1563, .T. ) ;
#12505 = DIRECTION ( 'NONE',  ( 1.445602896647339656E-16, -0.8212051873014208914, -0.5706330172266919076 ) ) ;
#12506 = EDGE_LOOP ( 'NONE', ( #18577, #8039, #3609, #15914 ) ) ;
#12507 = CARTESIAN_POINT ( 'NONE',  ( 39.64097644196145609, -21.75010033615993876, 75.81628532166148204 ) ) ;
#12508 = B_SPLINE_CURVE_WITH_KNOTS ( 'NONE', 3,
 ( #1100, #19150, #3432, #10787 ),
 .UNSPECIFIED., .F., .F.,
 ( 4, 4 ),
 ( 0.000000000000000000, 1.000000000000000000 ),
 .UNSPECIFIED. ) ;
#12509 = CARTESIAN_POINT ( 'NONE',  ( 46.81606138205707168, -37.70325315460876681, 65.37863370302704880 ) ) ;
#12510 = ORIENTED_EDGE ( 'NONE', *, *, #15871, .T. ) ;
#12511 = ORIENTED_EDGE ( 'NONE', *, *, #4827, .T. ) ;
#12512 = AXIS2_PLACEMENT_3D ( 'NONE', #10204, #19990, #19864 ) ;
#12513 = CARTESIAN_POINT ( 'NONE',  ( 37.61123632939164452, -19.70384086642190979, 69.02690120949091579 ) ) ;
#12514 = ADVANCED_FACE ( 'NONE', ( #19353 ), #13435, .T. ) ;
#12515 = CARTESIAN_POINT ( 'NONE',  ( 39.29254315202756231, -26.81368208888610027, 69.94417936956671156 ) ) ;
#12516 = CARTESIAN_POINT ( 'NONE',  ( 29.71606138205697789, -4.589472609077254184, -6.350807634294812765 ) ) ;
#12517 = FACE_OUTER_BOUND ( 'NONE', #1490, .T. ) ;
#12518 = CARTESIAN_POINT ( 'NONE',  ( 45.81606138205707168, -38.13418765192403015, 68.51141129791366780 ) ) ;
#12519 = ORIENTED_EDGE ( 'NONE', *, *, #4909, .T. ) ;
#12520 = AXIS2_PLACEMENT_3D ( 'NONE', #23685, #5322, #13904 ) ;
#12521 = FACE_OUTER_BOUND ( 'NONE', #17460, .T. ) ;
#12522 = FACE_OUTER_BOUND ( 'NONE', #1862, .T. ) ;
#12523 = CARTESIAN_POINT ( 'NONE',  ( 37.61123632939165873, -25.91368208888610880, 73.73360434286898624 ) ) ;
#12524 = FACE_OUTER_BOUND ( 'NONE', #3356, .T. ) ;
#12525 = PLANE ( 'NONE',  #4187 ) ;
#12526 =( GEOMETRIC_REPRESENTATION_CONTEXT ( 3 ) GLOBAL_UNCERTAINTY_ASSIGNED_CONTEXT ( ( #5397 ) ) GLOBAL_UNIT_ASSIGNED_CONTEXT ( ( #23294, #105, #4121 ) ) REPRESENTATION_CONTEXT ( 'NONE', 'WORKASPACE' ) );
#12527 = CARTESIAN_POINT ( 'NONE',  ( 39.29254315202756231, -10.81368208888610205, 69.94417936956673998 ) ) ;
#12528 = CARTESIAN_POINT ( 'NONE',  ( 29.81606138205707879, -39.99575152356569419, 63.13209164280871022 ) ) ;
#12529 = CARTESIAN_POINT ( 'NONE',  ( 39.82603832034401847, -18.31368208888610738, 72.40698646996131060 ) ) ;
#12530 = AXIS2_PLACEMENT_3D ( 'NONE', #11994, #20082, #9678 ) ;
#12531 = CARTESIAN_POINT ( 'NONE',  ( 45.81606138205697221, -4.589472609077215104, -6.350807634294792337 ) ) ;
#12532 = AXIS2_PLACEMENT_3D ( 'NONE', #2637, #6398, #698 ) ;
#12533 = DIRECTION ( 'NONE',  ( 0.000000000000000000, -1.000000000000000000, 0.000000000000000000 ) ) ;
#12534 = CARTESIAN_POINT ( 'NONE',  ( 37.89291511884479036, -22.50384086642191050, 72.49843995877330372 ) ) ;
#12535 = CARTESIAN_POINT ( 'NONE',  ( 38.26194895904383486, -13.01368208888610134, 69.64448340153877837 ) ) ;
#12536 = DIRECTION ( 'NONE',  ( -1.734723475976804876E-16, 0.8212051873014210024, 0.5706330172266920187 ) ) ;
#12537 = ORIENTED_EDGE ( 'NONE', *, *, #20926, .T. ) ;
#12538 = CARTESIAN_POINT ( 'NONE',  ( 38.93415946300896024, -11.50384086642190340, 69.66206559358663242 ) ) ;
#12539 = DIRECTION ( 'NONE',  ( -1.734723475976804876E-16, -3.491481338843135327E-15, -1.000000000000000000 ) ) ;
#12540 = AXIS2_PLACEMENT_3D ( 'NONE', #16921, #8690, #10494 ) ;
#12541 = ADVANCED_FACE ( 'NONE', ( #9207 ), #7388, .F. ) ;
#12542 = CARTESIAN_POINT ( 'NONE',  ( 39.29254315202756231, -2.813682088886101162, 69.94417936956673998 ) ) ;
#12543 = ORIENTED_EDGE ( 'NONE', *, *, #20502, .T. ) ;
#12544 = CARTESIAN_POINT ( 'NONE',  ( 36.36258059203031934, -13.71368208888610773, 72.86986841596736042 ) ) ;
#12545 = EDGE_LOOP ( 'NONE', ( #16687, #5458 ) ) ;
#12546 = CARTESIAN_POINT ( 'NONE',  ( 37.31606138205700063, 42.19123852234599781, 75.30501292736987295 ) ) ;
#12547 = CARTESIAN_POINT ( 'NONE',  ( 42.56606138205700063, 3.151453266960317023, 6.397347472316774031 ) ) ;
#12548 = CARTESIAN_POINT ( 'NONE',  ( 39.31564783533279694, -9.303840866421909439, 70.72433947564853440 ) ) ;
#12549 = CARTESIAN_POINT ( 'NONE',  ( 44.81606138205700063, 35.38401127291550097, 61.48364296169660292 ) ) ;
#12550 = EDGE_LOOP ( 'NONE', ( #24145, #10406, #5747, #7922 ) ) ;
#12551 = CARTESIAN_POINT ( 'NONE',  ( 40.81606138205700773, 37.44123852234599781, 75.30501292736990138 ) ) ;
#12552 = AXIS2_PLACEMENT_3D ( 'NONE', #21063, #9230, #5220 ) ;
#12553 = DIRECTION ( 'NONE',  ( 0.000000000000000000, 0.8191520442889929088, 0.5735764363510444941 ) ) ;
#12554 = CARTESIAN_POINT ( 'NONE',  ( 36.98690846071097127, -25.80384086642191477, 69.45876917294174291 ) ) ;
#12555 = DIRECTION ( 'NONE',  ( 0.000000000000000000, 1.000000000000000000, -2.999999999999999839E-15 ) ) ;
#12556 = CARTESIAN_POINT ( 'NONE',  ( 37.25202387243752611, -27.21368208888610241, 70.00779233799262613 ) ) ;
#12557 = DIRECTION ( 'NONE',  ( 1.734723475976804876E-16, 3.496552006265755350E-15, 1.000000000000000000 ) ) ;
#12558 = CARTESIAN_POINT ( 'NONE',  ( 43.31606138205700773, -18.80550481115970740, 25.27912300651437150 ) ) ;
#12559 = ADVANCED_FACE ( 'NONE', ( #21041 ), #17118, .T. ) ;
#12560 = VERTEX_POINT ( 'NONE', #21415 ) ;
#12561 = DIRECTION ( 'NONE',  ( 1.000000000000000275E-15, -0.9439899321577400748, -0.3299742535180970049 ) ) ;
#12562 = VERTEX_POINT ( 'NONE', #754 ) ;
#12563 = EDGE_CURVE ( 'NONE', #1030, #11095, #13725, .T. ) ;
#12564 = PLANE ( 'NONE',  #1102 ) ;
#12565 = CARTESIAN_POINT ( 'NONE',  ( 39.82603832034401137, -17.30384086642190411, 70.35351908239857721 ) ) ;
#12566 = DIRECTION ( 'NONE',  ( 1.000000000000000000, 0.000000000000000000, 0.000000000000000000 ) ) ;
#12567 = DIRECTION ( 'NONE',  ( 0.000000000000000000, 0.000000000000000000, -1.000000000000000000 ) ) ;
#12568 = ADVANCED_FACE ( 'NONE', ( #11767 ), #17682, .T. ) ;
#12569 = CARTESIAN_POINT ( 'NONE',  ( 40.31606138205700773, -10.66749763588699906, 14.47455635838400134 ) ) ;
#12570 = CARTESIAN_POINT ( 'NONE',  ( 43.31606138205700773, -19.34822312381089660, 24.15308711316412627 ) ) ;
#12571 = CARTESIAN_POINT ( 'NONE',  ( 36.68196826583682935, -28.00384086642191050, 70.79240656858105751 ) ) ;
#12572 = CARTESIAN_POINT ( 'NONE',  ( 38.31606138205700063, -5.204193249396280585, 82.80001292736993435 ) ) ;
#12573 = ORIENTED_EDGE ( 'NONE', *, *, #17282, .F. ) ;
#12574 = ADVANCED_FACE ( 'NONE', ( #21796 ), #23838, .F. ) ;
#12575 = CARTESIAN_POINT ( 'NONE',  ( 39.82603832034400426, -24.31368208888611093, 72.40698646996131060 ) ) ;
#12576 = ORIENTED_EDGE ( 'NONE', *, *, #24774, .F. ) ;
#12577 = EDGE_LOOP ( 'NONE', ( #16668, #23627 ) ) ;
#12578 = FACE_OUTER_BOUND ( 'NONE', #19875, .T. ) ;
#12579 = CARTESIAN_POINT ( 'NONE',  ( 37.31606138205700063, 16.19123852234700678, 71.30501292736995822 ) ) ;
#12580 = UNCERTAINTY_MEASURE_WITH_UNIT (LENGTH_MEASURE( 1.000000000000000082E-05 ), #1309, 'distance_accuracy_value', 'NONE');
#12581 = CARTESIAN_POINT ( 'NONE',  ( 39.02742774030102879, -4.213682088886099741, 72.26730301774236409 ) ) ;
#12582 = CARTESIAN_POINT ( 'NONE',  ( 39.37952058850012804, 1.386317911113897683, 70.97781676520604321 ) ) ;
#12583 = ORIENTED_EDGE ( 'NONE', *, *, #12356, .F. ) ;
#12584 = ORIENTED_EDGE ( 'NONE', *, *, #22873, .F. ) ;
#12585 = DIRECTION ( 'NONE',  ( 0.000000000000000000, -0.8967398287344631180, -0.4425581086832393041 ) ) ;
#12586 = CARTESIAN_POINT ( 'NONE',  ( 43.81606138205700063, 36.92314894770293421, 79.37823623207322044 ) ) ;
#12587 = LINE ( 'NONE', #3144, #18984 ) ;
#12588 = CARTESIAN_POINT ( 'NONE',  ( 36.68196826583682935, -12.00384086642191228, 70.79240656858107172 ) ) ;
#12589 = DIRECTION ( 'NONE',  ( 0.000000000000000000, -1.000000000000000000, 2.999999999999999839E-15 ) ) ;
#12590 = CARTESIAN_POINT ( 'NONE',  ( 36.81465384343994884, 41.43850569188389699, 79.87823623207322044 ) ) ;
#12591 = VERTEX_POINT ( 'NONE', #8140 ) ;
#12592 = ORIENTED_EDGE ( 'NONE', *, *, #5498, .F. ) ;
#12593 = FACE_OUTER_BOUND ( 'NONE', #6402, .T. ) ;
#12594 = EDGE_CURVE ( 'NONE', #2469, #16151, #17016, .T. ) ;
#12595 = CARTESIAN_POINT ( 'NONE',  ( 39.82603832034401847, -10.31368208888610560, 72.40698646996133903 ) ) ;
#12596 = LINE ( 'NONE', #4971, #3201 ) ;
#12597 = DIRECTION ( 'NONE',  ( -1.000000000000000000, -2.999999999999999839E-15, 0.000000000000000000 ) ) ;
#12598 = EDGE_CURVE ( 'NONE', #16335, #10282, #8785, .T. ) ;
#12599 = EDGE_CURVE ( 'NONE', #16389, #14611, #1943, .T. ) ;
#12600 = CARTESIAN_POINT ( 'NONE',  ( 43.27195111268100192, 2.993280262538516201, 6.111616072109399944 ) ) ;
#12601 = CARTESIAN_POINT ( 'NONE',  ( 34.56606138205700773, 47.04446929126260102, 82.37823623207320622 ) ) ;
#12602 = CARTESIAN_POINT ( 'NONE',  ( 37.44193150466009001, -5.391171257106773140, 82.80337612851013773 ) ) ;
#12603 = ADVANCED_FACE ( 'NONE', ( #7897 ), #17944, .T. ) ;
#12604 = FACE_OUTER_BOUND ( 'NONE', #2831, .T. ) ;
#12605 = ORIENTED_EDGE ( 'NONE', *, *, #23556, .T. ) ;
#12606 = EDGE_LOOP ( 'NONE', ( #724, #20535, #19282, #16425 ) ) ;
#12607 = CARTESIAN_POINT ( 'NONE',  ( 32.81606138205700773, 36.92314894770294131, 80.37823623207323465 ) ) ;
#12608 = CARTESIAN_POINT ( 'NONE',  ( 40.77203464402485622, -1.103840866421915035, 71.43714994484034264 ) ) ;
#12609 = CARTESIAN_POINT ( 'NONE',  ( 38.26194895904383486, -27.01368208888609956, 70.24448340153875847 ) ) ;
#12610 = ORIENTED_EDGE ( 'NONE', *, *, #13971, .T. ) ;
#12611 = ORIENTED_EDGE ( 'NONE', *, *, #9326, .T. ) ;
#12612 = CARTESIAN_POINT ( 'NONE',  ( 45.81606138205700063, 36.92314894770293421, 79.37823623207323465 ) ) ;
#12613 = CARTESIAN_POINT ( 'NONE',  ( 36.49096545463212493, -3.513682088886103116, 71.43714994484035685 ) ) ;
#12614 = CARTESIAN_POINT ( 'NONE',  ( 39.24876120206129571, 1.096159133578088696, 72.12822762946751709 ) ) ;
#12615 = DIRECTION ( 'NONE',  ( 0.000000000000000000, -1.000000000000000000, 4.382459307730880209E-15 ) ) ;
#12616 = EDGE_CURVE ( 'NONE', #17216, #2232, #9620, .T. ) ;
#12617 = CARTESIAN_POINT ( 'NONE',  ( 38.26194895904383486, -11.01368208888609956, 69.04448340153881247 ) ) ;
#12618 = CARTESIAN_POINT ( 'NONE',  ( 40.31606138205701484, -18.06006611532532702, 24.33356453583320445 ) ) ;
#12619 = CARTESIAN_POINT ( 'NONE',  ( 43.31606138205700063, 10.06218483883314718, 67.80501292737497465 ) ) ;
#12620 = DIRECTION ( 'NONE',  ( 0.000000000000000000, 1.000000000000000000, -3.469446951953614189E-15 ) ) ;
#12621 = FACE_OUTER_BOUND ( 'NONE', #10663, .T. ) ;
#12622 = APPLICATION_CONTEXT ( 'automotive_design' ) ;
#12623 = CARTESIAN_POINT ( 'NONE',  ( 43.69896204258590444, 3.548173818309682037, 6.215045287937394747 ) ) ;
#12624 = FACE_OUTER_BOUND ( 'NONE', #7844, .T. ) ;
#12625 = PLANE ( 'NONE',  #23830 ) ;
#12626 = CARTESIAN_POINT ( 'NONE',  ( 2.230251030284979743E-14, -5.575886420685237432, -6.837621553846413569 ) ) ;
#12627 = VERTEX_POINT ( 'NONE', #12272 ) ;
#12628 = ORIENTED_EDGE ( 'NONE', *, *, #20424, .F. ) ;
#12629 = UNCERTAINTY_MEASURE_WITH_UNIT (LENGTH_MEASURE( 1.000000000000000082E-05 ), #1909, 'distance_accuracy_value', 'NONE');
#12630 = CARTESIAN_POINT ( 'NONE',  ( 39.12911128074872380, -19.50384086642191406, 69.06206559358665231 ) ) ;
#12631 = CARTESIAN_POINT ( 'NONE',  ( 37.80618814713140097, -21.91368208888610880, 73.13360434286903455 ) ) ;
#12632 = FACE_OUTER_BOUND ( 'NONE', #18926, .T. ) ;
#12633 = EDGE_CURVE ( 'NONE', #14180, #17786, #23597, .T. ) ;
#12634 = EDGE_CURVE ( 'NONE', #4199, #6560, #12086, .T. ) ;
#12635 = CARTESIAN_POINT ( 'NONE',  ( 33.31606138205700773, -12.87480755223283424, 20.78922580900563588 ) ) ;
#12636 = CARTESIAN_POINT ( 'NONE',  ( 32.81606138205700773, 36.92314894770294131, 80.37823623207323465 ) ) ;
#12637 = ORIENTED_EDGE ( 'NONE', *, *, #21667, .T. ) ;
#12638 = CARTESIAN_POINT ( 'NONE',  ( 39.31606138205700063, 43.19123852234599781, 74.30501292736987295 ) ) ;
#12639 = CARTESIAN_POINT ( 'NONE',  ( 38.26194895904384907, 1.396159133578083633, 73.11602215082119471 ) ) ;
#12640 = CARTESIAN_POINT ( 'NONE',  ( 36.29569395875881099, -0.3038408664219164890, 72.77780686321129622 ) ) ;
#12641 = AXIS2_PLACEMENT_3D ( 'NONE', #10896, #13217, #1213 ) ;
#12642 = ORIENTED_EDGE ( 'NONE', *, *, #24380, .F. ) ;
#12643 = CARTESIAN_POINT ( 'NONE',  ( 43.31606138205700773, -19.47805968271054766, 24.94720442500192448 ) ) ;
#12644 = CARTESIAN_POINT ( 'NONE',  ( 29.81606138205705037, -30.65246816789535345, 72.44500581826353880 ) ) ;
#12645 = CIRCLE ( 'NONE', #9772, 1.000000000000000888 ) ;
#12646 = AXIS2_PLACEMENT_3D ( 'NONE', #24094, #8667, #10849 ) ;
#12647 = CARTESIAN_POINT ( 'NONE',  ( 36.64852494920107517, -1.413682088886102806, 70.89533451361948835 ) ) ;
#12648 = CARTESIAN_POINT ( 'NONE',  ( 36.81606138205700063, -7.086900875803856970, 56.51273394326043586 ) ) ;
#12649 = CARTESIAN_POINT ( 'NONE',  ( 38.82593461698262871, -18.91368208888609814, 69.62690120949091011 ) ) ;
#12650 = LINE ( 'NONE', #20368, #13941 ) ;
#12651 = EDGE_CURVE ( 'NONE', #546, #9564, #18651, .T. ) ;
#12652 = CARTESIAN_POINT ( 'NONE',  ( 43.23147868389327897, 42.57231754924293909, 79.57823623207323749 ) ) ;
#12653 = CARTESIAN_POINT ( 'NONE',  ( 39.02742774030101458, -21.40384086642191619, 70.49320253461759478 ) ) ;
#12654 = CARTESIAN_POINT ( 'NONE',  ( 38.26194895904383486, -5.013682088886102228, 69.64448340153879258 ) ) ;
#12655 = LINE ( 'NONE', #6710, #18905 ) ;
#12656 = EDGE_LOOP ( 'NONE', ( #12378, #9469, #15312, #25448 ) ) ;
#12657 = CARTESIAN_POINT ( 'NONE',  ( 37.69796330110505522, -6.503840866421914058, 73.09843995877331224 ) ) ;
#12658 = LINE ( 'NONE', #18326, #2335 ) ;
#12659 = AXIS2_PLACEMENT_3D ( 'NONE', #2856, #11258, #24487 ) ;
#12660 = AXIS2_PLACEMENT_3D ( 'NONE', #13382, #21226, #19285 ) ;
#12661 = CARTESIAN_POINT ( 'NONE',  ( 36.49096545463212493, -7.513682088886102228, 71.43714994484035685 ) ) ;
#12662 = ORIENTED_EDGE ( 'NONE', *, *, #9650, .T. ) ;
#12663 = CARTESIAN_POINT ( 'NONE',  ( 39.02088643472237095, -10.91368208888610170, 69.02690120949094421 ) ) ;
#12664 = ORIENTED_EDGE ( 'NONE', *, *, #14290, .T. ) ;
#12665 = DIRECTION ( 'NONE',  ( 1.000000000000000000, 0.000000000000000000, 0.000000000000000000 ) ) ;
#12666 = DIRECTION ( 'NONE',  ( 1.000000000000000000, 0.000000000000000000, 0.000000000000000000 ) ) ;
#12667 = CARTESIAN_POINT ( 'NONE',  ( 38.26194895904384197, -12.60384086642191015, 72.51602215082118619 ) ) ;
#12668 = CARTESIAN_POINT ( 'NONE',  ( 43.81606138205700063, -3.566646240838321269, 18.16837712155798457 ) ) ;
#12669 = ORIENTED_EDGE ( 'NONE', *, *, #2690, .F. ) ;
#12670 = DIRECTION ( 'NONE',  ( -1.000000000000000000, -4.029870553924695461E-16, 4.592402829583201910E-16 ) ) ;
#12671 = CARTESIAN_POINT ( 'NONE',  ( 43.31606138205700773, -19.92642959707777806, 24.72592537066031682 ) ) ;
#12672 = CARTESIAN_POINT ( 'NONE',  ( 38.37017380507018771, -17.60384086642191193, 69.04448340153878405 ) ) ;
#12673 = CARTESIAN_POINT ( 'NONE',  ( 38.31606138205700063, 15.19123852234700500, 71.30501292736995822 ) ) ;
#12674 = FACE_OUTER_BOUND ( 'NONE', #12453, .T. ) ;
#12675 = CARTESIAN_POINT ( 'NONE',  ( 39.95015449827720744, -20.61368208888610454, 70.79240656858105751 ) ) ;
#12676 = DIRECTION ( 'NONE',  ( -1.000000000000000000, 5.204170427930413997E-31, 1.734723475976804876E-16 ) ) ;
#12677 = CARTESIAN_POINT ( 'NONE',  ( 44.81606138205700063, -34.55876147765400930, 73.30501292737011454 ) ) ;
#12678 = AXIS2_PLACEMENT_3D ( 'NONE', #8011, #15848, #10185 ) ;
#12679 = ORIENTED_EDGE ( 'NONE', *, *, #4994, .T. ) ;
#12680 = AXIS2_PLACEMENT_3D ( 'NONE', #16111, #8883, #14791 ) ;
#12681 = CARTESIAN_POINT ( 'NONE',  ( 32.81606138205700773, -35.41471100349711065, 71.53682070832086026 ) ) ;
#12682 = CARTESIAN_POINT ( 'NONE',  ( 32.81606138205700773, -37.34243788671330577, 70.80615726751818784 ) ) ;
#12683 = EDGE_CURVE ( 'NONE', #11586, #20703, #13688, .T. ) ;
#12684 = CARTESIAN_POINT ( 'NONE',  ( 39.98359781491296161, -17.20384086642190979, 70.89533451361945993 ) ) ;
#12685 = CARTESIAN_POINT ( 'NONE',  ( 0.000000000000000000, 0.000000000000000000, 0.000000000000000000 ) ) ;
#12686 = FACE_OUTER_BOUND ( 'NONE', #605, .T. ) ;
#12687 = VERTEX_POINT ( 'NONE', #14066 ) ;
#12688 = CARTESIAN_POINT ( 'NONE',  ( 35.64099152588522657, 1.142818861812999742, 82.55501292736997243 ) ) ;
#12689 = LINE ( 'NONE', #5420, #20993 ) ;
#12690 = CARTESIAN_POINT ( 'NONE',  ( 37.25202387243754032, -26.40384086642191619, 72.75271321436730432 ) ) ;
#12691 = CARTESIAN_POINT ( 'NONE',  ( 36.80507328770344344, -5.854377449151428436, 82.77924324848135029 ) ) ;
#12692 = ORIENTED_EDGE ( 'NONE', *, *, #7029, .T. ) ;
#12693 = CARTESIAN_POINT ( 'NONE',  ( 39.98359781491296161, -26.41368208888610525, 71.86517103874045631 ) ) ;
#12694 = VERTEX_POINT ( 'NONE', #23966 ) ;
#12695 = ORIENTED_EDGE ( 'NONE', *, *, #5485, .F. ) ;
#12696 = VECTOR ( 'NONE', #22623, 1000.000000000000114 ) ;
#12697 = DIRECTION ( 'NONE',  ( 1.000000000000000000, 0.000000000000000000, 0.000000000000000000 ) ) ;
#12698 = FACE_OUTER_BOUND ( 'NONE', #18599, .T. ) ;
#12699 = CARTESIAN_POINT ( 'NONE',  ( 37.25260217561390874, -28.00384086642191406, 70.97781676520601479 ) ) ;
#12700 = AXIS2_PLACEMENT_3D ( 'NONE', #7321, #15428, #1754 ) ;
#12701 = CARTESIAN_POINT ( 'NONE',  ( 37.60469502381300089, 0.7863179111138978161, 70.49320253461759478 ) ) ;
#12702 = VERTEX_POINT ( 'NONE', #6341 ) ;
#12703 = EDGE_LOOP ( 'NONE', ( #8075, #22847, #2907, #11842 ) ) ;
#12704 = DIRECTION ( 'NONE',  ( -1.327674326049719602E-15, 0.4425581086832399147, -0.8967398287344627850 ) ) ;
#12705 = DIRECTION ( 'NONE',  ( 2.312964634635742267E-15, -0.8967398287344627850, -0.4425581086832398592 ) ) ;
#12706 =( LENGTH_UNIT ( ) NAMED_UNIT ( * ) SI_UNIT ( .MILLI., .METRE. ) );
#12707 = CARTESIAN_POINT ( 'NONE',  ( 39.75915168707251723, -4.903840866421914413, 72.49904802271740323 ) ) ;
#12708 = CARTESIAN_POINT ( 'NONE',  ( 43.31606138205700063, -10.66749763588699551, 14.47455635838400134 ) ) ;
#12709 = ORIENTED_EDGE ( 'NONE', *, *, #523, .F. ) ;
#12710 = MECHANICAL_DESIGN_GEOMETRIC_PRESENTATION_REPRESENTATION (  '', ( #22987 ), #6937 ) ;
#12711 = ORIENTED_EDGE ( 'NONE', *, *, #21435, .T. ) ;
#12712 = LINE ( 'NONE', #24779, #13695 ) ;
#12713 = CARTESIAN_POINT ( 'NONE',  ( 36.68196826583682935, -1.613682088886104982, 71.96809898377890136 ) ) ;
#12714 = EDGE_CURVE ( 'NONE', #59, #1002, #7573, .T. ) ;
#12715 = ORIENTED_EDGE ( 'NONE', *, *, #7939, .T. ) ;
#12716 = FACE_OUTER_BOUND ( 'NONE', #2111, .T. ) ;
#12717 = DIRECTION ( 'NONE',  ( 0.000000000000000000, 0.5706330172266919076, -0.8212051873014208914 ) ) ;
#12718 = VECTOR ( 'NONE', #21417, 1000.000000000000000 ) ;
#12719 = DIRECTION ( 'NONE',  ( 1.734723475976807094E-15, -0.7516416929448819229, -0.6595716529892350355 ) ) ;
#12720 = CARTESIAN_POINT ( 'NONE',  ( 43.31606138205700063, -5.204193249396280585, 82.80501292736992980 ) ) ;
#12721 = CARTESIAN_POINT ( 'NONE',  ( 38.18583742984269946, -5.204226263507460537, 82.80501292736992980 ) ) ;
#12722 = VECTOR ( 'NONE', #16884, 1000.000000000000114 ) ;
#12723 = DIRECTION ( 'NONE',  ( 1.000000000000000000, 6.938893903907222067E-15, 0.000000000000000000 ) ) ;
#12724 = VERTEX_POINT ( 'NONE', #15866 ) ;
#12725 = ORIENTED_EDGE ( 'NONE', *, *, #584, .F. ) ;
#12726 = CARTESIAN_POINT ( 'NONE',  ( 45.81606138205697931, -6.382952266546142006, -7.235923851661271833 ) ) ;
#12727 = AXIS2_PLACEMENT_3D ( 'NONE', #863, #10937, #10806 ) ;
#12728 = DIRECTION ( 'NONE',  ( 1.000000000000000000, -1.115179377413661005E-30, -3.717264591378870232E-16 ) ) ;
#12729 = EDGE_CURVE ( 'NONE', #14052, #24921, #21543, .T. ) ;
#12730 = ADVANCED_FACE ( 'NONE', ( #13940 ), #4155, .F. ) ;
#12731 = CARTESIAN_POINT ( 'NONE',  ( 39.31564783533280405, -20.31368208888610027, 72.03616607671141026 ) ) ;
#12732 = ORIENTED_EDGE ( 'NONE', *, *, #19178, .T. ) ;
#12733 = ORIENTED_EDGE ( 'NONE', *, *, #2194, .F. ) ;
#12734 = FACE_OUTER_BOUND ( 'NONE', #12656, .T. ) ;
#12735 = CARTESIAN_POINT ( 'NONE',  ( 39.75915168707250302, -4.713682088886100630, 70.26145752964252722 ) ) ;
#12736 = CARTESIAN_POINT ( 'NONE',  ( 36.64852494920107517, -28.20384086642191335, 71.86517103874047052 ) ) ;
#12737 = EDGE_CURVE ( 'NONE', #13774, #17582, #20994, .T. ) ;
#12738 = EDGE_CURVE ( 'NONE', #20175, #2245, #4678, .T. ) ;
#12739 = ADVANCED_FACE ( 'NONE', ( #24088 ), #20491, .T. ) ;
#12740 = AXIS2_PLACEMENT_3D ( 'NONE', #20119, #522, #8407 ) ;
#12741 = DIRECTION ( 'NONE',  ( 0.000000000000000000, 1.000000000000000000, -2.999999999999999839E-15 ) ) ;
#12742 = CARTESIAN_POINT ( 'NONE',  ( 40.77203464402485622, -6.513682088886103116, 71.32335560751961623 ) ) ;
#12743 = CIRCLE ( 'NONE', #3242, 2.499999999999998668 ) ;
#12744 = LINE ( 'NONE', #7056, #1211 ) ;
#12745 = FACE_OUTER_BOUND ( 'NONE', #2513, .T. ) ;
#12746 = EDGE_CURVE ( 'NONE', #8428, #21357, #2825, .T. ) ;
#12747 = DIRECTION ( 'NONE',  ( 1.000000000000000000, 1.734723475976804876E-16, -1.734723475976814737E-16 ) ) ;
#12748 = ADVANCED_FACE ( 'NONE', ( #6834 ), #20757, .F. ) ;
#12749 = CARTESIAN_POINT ( 'NONE',  ( 36.31606138205700063, 8.691238522346987239, 65.30501292736998664 ) ) ;
#12750 = CIRCLE ( 'NONE', #23424, 2.500000000000002220 ) ;
#12751 = CARTESIAN_POINT ( 'NONE',  ( 43.14077072142541169, 3.506326161111083195, 6.337847826736607182 ) ) ;
#12752 = CARTESIAN_POINT ( 'NONE',  ( 43.31606138205700063, 6.289375473607850431, 7.138843309009015314 ) ) ;
#12753 = DIRECTION ( 'NONE',  ( 0.000000000000000000, 0.5706330172266919076, -0.8212051873014208914 ) ) ;
#12754 = AXIS2_PLACEMENT_3D ( 'NONE', #11333, #3192, #1003 ) ;
#12755 = ORIENTED_EDGE ( 'NONE', *, *, #13102, .F. ) ;
#12756 = CARTESIAN_POINT ( 'NONE',  ( 38.96215273200666473, -22.11857000840811693, 75.30036226159070623 ) ) ;
#12757 = CARTESIAN_POINT ( 'NONE',  ( 40.31606138205700063, 5.691238522346989903, 65.80501292736998664 ) ) ;
#12758 = VERTEX_POINT ( 'NONE', #20623 ) ;
#12759 = ORIENTED_EDGE ( 'NONE', *, *, #1395, .T. ) ;
#12760 = CARTESIAN_POINT ( 'NONE',  ( 36.29569395875881099, -18.30384086642191477, 72.77780686321128201 ) ) ;
#12761 = AXIS2_PLACEMENT_3D ( 'NONE', #16408, #4329, #24256 ) ;
#12762 = CARTESIAN_POINT ( 'NONE',  ( 37.33957961208646736, -19.81368208888611093, 72.81632618279321889 ) ) ;
#12763 = CARTESIAN_POINT ( 'NONE',  ( 32.81606138205700773, 36.92314894770293421, 79.37823623207323465 ) ) ;
#12764 = AXIS2_PLACEMENT_3D ( 'NONE', #23754, #5995, #1980 ) ;
#12765 = DIRECTION ( 'NONE',  ( 0.000000000000000000, 0.3299742535180974490, -0.9439899321577398528 ) ) ;
#12766 = DIRECTION ( 'NONE',  ( 0.000000000000000000, 0.000000000000000000, 1.000000000000000000 ) ) ;
#12767 = VERTEX_POINT ( 'NONE', #18562 ) ;
#12768 = LINE ( 'NONE', #2942, #1447 ) ;
#12769 = DIRECTION ( 'NONE',  ( 1.734723475976814737E-16, 0.000000000000000000, 1.000000000000000000 ) ) ;
#12770 = CARTESIAN_POINT ( 'NONE',  ( 36.98690846071097837, -27.81368208888610738, 73.30173637941817333 ) ) ;
#12771 = ORIENTED_EDGE ( 'NONE', *, *, #12959, .F. ) ;
#12772 = DIRECTION ( 'NONE',  ( 0.000000000000000000, 0.1918498038142811835, -0.9814242980364923374 ) ) ;
#12773 = LINE ( 'NONE', #16743, #4209 ) ;
#12774 = CARTESIAN_POINT ( 'NONE',  ( 37.33957961208646736, -3.813682088886109156, 72.81632618279323310 ) ) ;
#12775 = DIRECTION ( 'NONE',  ( 0.000000000000000000, 0.3299742535180969494, -0.9439899321577399638 ) ) ;
#12776 = CARTESIAN_POINT ( 'NONE',  ( 36.49096545463212493, -17.51368208888610667, 71.43714994484034264 ) ) ;
#12777 = AXIS2_PLACEMENT_3D ( 'NONE', #1665, #7486, #7749 ) ;
#12778 = LINE ( 'NONE', #24333, #15168 ) ;
#12779 = DIRECTION ( 'NONE',  ( 0.000000000000000000, 1.000000000000000000, -4.625929269271481378E-15 ) ) ;
#12780 = AXIS2_PLACEMENT_3D ( 'NONE', #3701, #23535, #7974 ) ;
#12781 = CARTESIAN_POINT ( 'NONE',  ( 38.73920764526923932, -17.50384086642191406, 70.26206559358661252 ) ) ;
#12782 = CARTESIAN_POINT ( 'NONE',  ( 40.14115730948191185, -6.513682088886103116, 71.32335560751961623 ) ) ;
#12783 = LINE ( 'NONE', #10843, #2028 ) ;
#12784 = ORIENTED_EDGE ( 'NONE', *, *, #23886, .T. ) ;
#12785 = CARTESIAN_POINT ( 'NONE',  ( 39.29254315202757653, -2.803840866421915212, 72.81632618279323310 ) ) ;
#12786 = LINE ( 'NONE', #8409, #10998 ) ;
#12787 = CARTESIAN_POINT ( 'NONE',  ( 38.82593461698262871, -6.913682088886100807, 69.62690120949091011 ) ) ;
#12788 = EDGE_LOOP ( 'NONE', ( #25295, #7590, #23846, #24353 ) ) ;
#12789 = CARTESIAN_POINT ( 'NONE',  ( 36.29569395875879678, -9.313682088886098498, 69.98269868914869107 ) ) ;
#12790 = ORIENTED_EDGE ( 'NONE', *, *, #22005, .F. ) ;
#12791 = CARTESIAN_POINT ( 'NONE',  ( 32.81606138205700773, -24.55876147765401285, 70.30501292737008612 ) ) ;
#12792 = CARTESIAN_POINT ( 'NONE',  ( 39.24876120206129571, -10.90384086642191264, 72.12822762946750288 ) ) ;
#12793 = DIRECTION ( 'NONE',  ( -9.027796614315171564E-31, -1.000000000000000000, -3.938893903907230117E-15 ) ) ;
#12794 = AXIS2_PLACEMENT_3D ( 'NONE', #12326, #10255, #21972 ) ;
#12795 = ORIENTED_EDGE ( 'NONE', *, *, #5924, .F. ) ;
#12796 = CARTESIAN_POINT ( 'NONE',  ( 41.31606138205687273, 43.19123852234595518, 61.80501292736988006 ) ) ;
#12797 = FACE_OUTER_BOUND ( 'NONE', #218, .T. ) ;
#12798 = CARTESIAN_POINT ( 'NONE',  ( 40.33642880535521869, -17.30384086642191477, 69.98269868914866265 ) ) ;
#12799 = CARTESIAN_POINT ( 'NONE',  ( 37.31068429205632953, -21.96856463034017892, 75.80811620457531319 ) ) ;
#12800 = CARTESIAN_POINT ( 'NONE',  ( 40.14115730948191185, -22.51368208888609956, 71.32335560751960202 ) ) ;
#12801 = DIRECTION ( 'NONE',  ( 1.000000000000000000, -3.009265538105074850E-31, -1.734723475976809806E-16 ) ) ;
#12802 = PLANE ( 'NONE',  #17217 ) ;
#12803 = ORIENTED_EDGE ( 'NONE', *, *, #21482, .F. ) ;
#12804 = FACE_OUTER_BOUND ( 'NONE', #5418, .T. ) ;
#12805 = CARTESIAN_POINT ( 'NONE',  ( 40.31606138205700063, 8.691238522346989015, 65.80501292736998664 ) ) ;
#12806 = CARTESIAN_POINT ( 'NONE',  ( 38.82593461698264292, -12.70384086642191512, 73.13360434286903455 ) ) ;
#12807 = CARTESIAN_POINT ( 'NONE',  ( 0.000000000000000000, 0.000000000000000000, 0.000000000000000000 ) ) ;
#12808 = ADVANCED_FACE ( 'NONE', ( #10460, #3090, #1025 ), #8909, .T. ) ;
#12809 = DIRECTION ( 'NONE',  ( -1.000000000000000000, -1.734723475976814737E-16, 8.024708101613549867E-31 ) ) ;
#12810 = CARTESIAN_POINT ( 'NONE',  ( 39.82603832034400426, -26.31368208888611093, 72.40698646996131060 ) ) ;
#12811 = EDGE_CURVE ( 'NONE', #10286, #3155, #3027, .T. ) ;
#12812 = DIRECTION ( 'NONE',  ( 0.000000000000000000, -0.7540134720837724513, -0.6568589528324737525 ) ) ;
#12813 = VECTOR ( 'NONE', #23514, 1000.000000000000000 ) ;
#12814 = DIRECTION ( 'NONE',  ( -1.000000000000000000, -1.052872940142565459E-15, -1.848188032574765003E-17 ) ) ;
#12815 = CARTESIAN_POINT ( 'NONE',  ( 37.69796330110505522, -24.50384086642190695, 73.09843995877328382 ) ) ;
#12816 = CARTESIAN_POINT ( 'NONE',  ( 36.37840728046802496, -20.80772986314774187, 75.90997265879607880 ) ) ;
#12817 = CARTESIAN_POINT ( 'NONE',  ( 37.33957961208646736, -21.81368208888610738, 72.81632618279321889 ) ) ;
#12818 = ORIENTED_EDGE ( 'NONE', *, *, #2878, .F. ) ;
#12819 = ORIENTED_EDGE ( 'NONE', *, *, #21686, .F. ) ;
#12820 = DIRECTION ( 'NONE',  ( -1.734723475976804876E-16, 1.000000000000000000, 0.000000000000000000 ) ) ;
#12821 = CYLINDRICAL_SURFACE ( 'NONE', #22744, 1.499999999999999778 ) ;
#12822 = CARTESIAN_POINT ( 'NONE',  ( 37.21915885897815457, 0.5863179111138989708, 71.08074471024443142 ) ) ;
#12823 = CARTESIAN_POINT ( 'NONE',  ( 38.00113996487114321, 0.08631791111389855442, 72.53360434286905445 ) ) ;
#12824 = ORIENTED_EDGE ( 'NONE', *, *, #24180, .F. ) ;
#12825 = VERTEX_POINT ( 'NONE', #24462 ) ;
#12826 = CYLINDRICAL_SURFACE ( 'NONE', #7592, 0.2000000000000057288 ) ;
#12827 = EDGE_CURVE ( 'NONE', #23772, #1612, #6336, .T. ) ;
#12828 = LINE ( 'NONE', #24637, #23572 ) ;
#12829 = VERTEX_POINT ( 'NONE', #18813 ) ;
#12830 = PRESENTATION_STYLE_ASSIGNMENT (( #24515 ) ) ;
#12831 = CARTESIAN_POINT ( 'NONE',  ( 36.64852494920107517, -6.203840866421912459, 71.86517103874049894 ) ) ;
#12832 = SPHERICAL_SURFACE ( 'NONE', #10059, 2.000000000000000000 ) ;
#12833 = DIRECTION ( 'NONE',  ( -1.000000000000000000, 0.000000000000000000, 0.000000000000000000 ) ) ;
#12834 = ORIENTED_EDGE ( 'NONE', *, *, #5900, .T. ) ;
#12835 = ORIENTED_EDGE ( 'NONE', *, *, #6030, .T. ) ;
#12836 = VERTEX_POINT ( 'NONE', #22170 ) ;
#12837 = DIRECTION ( 'NONE',  ( 1.000000000000000000, 2.999999999999999839E-15, -5.603103565922875308E-33 ) ) ;
#12838 = CARTESIAN_POINT ( 'NONE',  ( 36.64852494920107517, 0.5863179111138955291, 70.89533451361948835 ) ) ;
#12839 = AXIS2_PLACEMENT_3D ( 'NONE', #21943, #10608, #18091 ) ;
#12840 = CARTESIAN_POINT ( 'NONE',  ( 46.81606138205697221, -3.984974717493081187, -3.847356352999882656 ) ) ;
#12841 = DIRECTION ( 'NONE',  ( -1.000000000000000000, -1.734723475976804876E-16, 1.734723475976814737E-16 ) ) ;
#12842 = DIRECTION ( 'NONE',  ( 1.734723475976804876E-16, -1.000000000000000000, -3.009265538105065326E-32 ) ) ;
#12843 = DIRECTION ( 'NONE',  ( 0.000000000000000000, 1.000000000000000000, -3.469446951953614189E-15 ) ) ;
#12844 = CARTESIAN_POINT ( 'NONE',  ( 43.31606138205700063, -10.19550266980812658, 14.63954348514304904 ) ) ;
#12845 = FACE_OUTER_BOUND ( 'NONE', #11401, .T. ) ;
#12846 = ORIENTED_EDGE ( 'NONE', *, *, #7743, .T. ) ;
#12847 = ORIENTED_EDGE ( 'NONE', *, *, #10782, .T. ) ;
#12848 = VECTOR ( 'NONE', #23541, 1000.000000000000000 ) ;
#12849 = DIRECTION ( 'NONE',  ( 0.000000000000000000, -0.8212051873014213355, -0.5706330172266915746 ) ) ;
#12850 = LINE ( 'NONE', #3433, #24657 ) ;
#12851 = CARTESIAN_POINT ( 'NONE',  ( 37.21915885897815457, -15.41368208888610347, 71.08074471024443142 ) ) ;
#12852 = ORIENTED_EDGE ( 'NONE', *, *, #23409, .F. ) ;
#12853 = ORIENTED_EDGE ( 'NONE', *, *, #1582, .F. ) ;
#12854 = EDGE_CURVE ( 'NONE', #874, #546, #639, .T. ) ;
#12855 = VECTOR ( 'NONE', #15150, 1000.000000000000000 ) ;
#12856 = DIRECTION ( 'NONE',  ( -8.791731484610113542E-17, 0.9135454576426023099, 0.4067366430757970996 ) ) ;
#12857 = CARTESIAN_POINT ( 'NONE',  ( 39.29254315202756231, -4.813682088886099386, 69.94417936956673998 ) ) ;
#12858 = CARTESIAN_POINT ( 'NONE',  ( 38.82593461698265003, -22.70384086642191690, 73.13360434286903455 ) ) ;
#12859 = DIRECTION ( 'NONE',  ( 0.000000000000000000, 0.000000000000000000, 1.000000000000000000 ) ) ;
#12860 = CARTESIAN_POINT ( 'NONE',  ( 38.37017380507020192, -10.01368208888611022, 73.71602215082116061 ) ) ;
#12861 = DIRECTION ( 'NONE',  ( 0.000000000000000000, 0.6568589528324746407, -0.7540134720837716742 ) ) ;
#12862 = VERTEX_POINT ( 'NONE', #22422 ) ;
#12863 = DIRECTION ( 'NONE',  ( 0.000000000000000000, -0.8212051873014288850, -0.5706330172266804723 ) ) ;
#12864 = DIRECTION ( 'NONE',  ( 1.734723475976805122E-16, 3.491481338843134933E-15, 1.000000000000000000 ) ) ;
#12865 = LINE ( 'NONE', #3184, #9161 ) ;
#12866 = EDGE_CURVE ( 'NONE', #6369, #16802, #4773, .T. ) ;
#12867 = ADVANCED_FACE ( 'NONE', ( #8659 ), #2700, .F. ) ;
#12868 = CARTESIAN_POINT ( 'NONE',  ( 40.31606138205700773, -6.984952308121978426, 82.64599116981820259 ) ) ;
#12869 = CARTESIAN_POINT ( 'NONE',  ( 33.31606138205700773, -10.80800258567212602, 32.62011605800211811 ) ) ;
#12870 = AXIS2_PLACEMENT_3D ( 'NONE', #16165, #12200, #21973 ) ;
#12871 = EDGE_CURVE ( 'NONE', #25303, #10220, #6734, .T. ) ;
#12872 = EDGE_CURVE ( 'NONE', #13140, #20940, #24584, .T. ) ;
#12873 = PLANE ( 'NONE',  #18070 ) ;
#12874 = EDGE_CURVE ( 'NONE', #22990, #15655, #12925, .T. ) ;
#12875 = ORIENTED_EDGE ( 'NONE', *, *, #22325, .T. ) ;
#12876 = CARTESIAN_POINT ( 'NONE',  ( 45.81606138205707168, -38.13418765192403015, 68.51141129791366780 ) ) ;
#12877 = CARTESIAN_POINT ( 'NONE',  ( 40.81606138205700773, -31.05876147765399864, 74.30501292737010033 ) ) ;
#12878 = ORIENTED_EDGE ( 'NONE', *, *, #22491, .T. ) ;
#12879 = AXIS2_PLACEMENT_3D ( 'NONE', #2413, #14275, #9915 ) ;
#12880 = ORIENTED_EDGE ( 'NONE', *, *, #15581, .T. ) ;
#12881 = UNCERTAINTY_MEASURE_WITH_UNIT (LENGTH_MEASURE( 1.000000000000000082E-05 ), #19182, 'distance_accuracy_value', 'NONE');
#12882 = CARTESIAN_POINT ( 'NONE',  ( 36.07789103942399578, -16.20384086642191690, 72.05058123536544201 ) ) ;
#12883 = EDGE_CURVE ( 'NONE', #3532, #19706, #6966, .T. ) ;
#12884 = AXIS2_PLACEMENT_3D ( 'NONE', #18461, #13871, #4797 ) ;
#12885 = CARTESIAN_POINT ( 'NONE',  ( 38.37017380507020192, -22.01368208888611022, 73.11602215082116629 ) ) ;
#12886 = LINE ( 'NONE', #1134, #24293 ) ;
#12887 = CIRCLE ( 'NONE', #7943, 0.2314957320545540931 ) ;
#12888 = DIRECTION ( 'NONE',  ( -1.000000000000000078E-15, 0.9439899321577400748, 0.3299742535180970049 ) ) ;
#12889 = VERTEX_POINT ( 'NONE', #15452 ) ;
#12890 = CYLINDRICAL_SURFACE ( 'NONE', #19956, 1.000000000000000888 ) ;
#12891 = DIRECTION ( 'NONE',  ( 0.000000000000000000, -6.938893903907222067E-15, -1.000000000000000000 ) ) ;
#12892 = AXIS2_PLACEMENT_3D ( 'NONE', #23227, #7530, #2094 ) ;
#12893 = CARTESIAN_POINT ( 'NONE',  ( 39.64521430340304420, -26.81368208888610738, 69.45876917294174291 ) ) ;
#12894 = ORIENTED_EDGE ( 'NONE', *, *, #3718, .T. ) ;
#12895 = CARTESIAN_POINT ( 'NONE',  ( 43.81606138205700063, 41.44123852234599070, 73.55501292736987295 ) ) ;
#12896 = DIRECTION ( 'NONE',  ( 0.000000000000000000, 1.000000000000000000, -3.469446951953613400E-15 ) ) ;
#12897 = CARTESIAN_POINT ( 'NONE',  ( 36.49096545463212493, 0.4863179111138959954, 71.43714994484035685 ) ) ;
#12898 = DIRECTION ( 'NONE',  ( 0.000000000000000000, -1.000000000000000000, 2.999999999999999839E-15 ) ) ;
#12899 = CIRCLE ( 'NONE', #14524, 1.000000000000000888 ) ;
#12900 = CARTESIAN_POINT ( 'NONE',  ( 36.49096545463212493, -23.51368208888609956, 71.43714994484031422 ) ) ;
#12901 = DIRECTION ( 'NONE',  ( 0.000000000000000000, 0.4425581086832399702, -0.8967398287344626739 ) ) ;
#12902 = DIRECTION ( 'NONE',  ( 0.000000000000000000, 0.000000000000000000, -1.000000000000000000 ) ) ;
#12903 = EDGE_CURVE ( 'NONE', #17183, #18894, #17264, .T. ) ;
#12904 = CARTESIAN_POINT ( 'NONE',  ( 37.12184278917507640, -22.10384086642191193, 71.32335560751961623 ) ) ;
#12905 = CARTESIAN_POINT ( 'NONE',  ( 36.80608444377001121, -5.313682088886100274, 70.35351908239860563 ) ) ;
#12906 = EDGE_CURVE ( 'NONE', #5182, #21232, #1785, .T. ) ;
#12907 = ORIENTED_EDGE ( 'NONE', *, *, #20364, .F. ) ;
#12908 = FACE_OUTER_BOUND ( 'NONE', #11332, .T. ) ;
#12909 = CIRCLE ( 'NONE', #3448, 1.000000000000000888 ) ;
#12910 = ORIENTED_EDGE ( 'NONE', *, *, #1180, .F. ) ;
#12911 = CARTESIAN_POINT ( 'NONE',  ( 36.49096545463212493, -6.103840866421912814, 71.32335560751963044 ) ) ;
#12912 = DIRECTION ( 'NONE',  ( 0.000000000000000000, -3.491481338843135327E-15, -1.000000000000000000 ) ) ;
#12913 = AXIS2_PLACEMENT_3D ( 'NONE', #2482, #12179, #16015 ) ;
#12914 = CARTESIAN_POINT ( 'NONE',  ( 39.75915168707250302, -4.713682088886100630, 70.26145752964252722 ) ) ;
#12915 = ORIENTED_EDGE ( 'NONE', *, *, #8860, .T. ) ;
#12916 = CARTESIAN_POINT ( 'NONE',  ( 36.11133435605973574, -11.61368208888610454, 72.15350918040385864 ) ) ;
#12917 = ORIENTED_EDGE ( 'NONE', *, *, #17904, .T. ) ;
#12918 = DIRECTION ( 'NONE',  ( -1.000000000000000000, -2.896293624483393641E-15, 5.118106270778061927E-17 ) ) ;
#12919 = CARTESIAN_POINT ( 'NONE',  ( 37.25260217561390874, -12.00384086642191228, 70.97781676520601479 ) ) ;
#12920 = DIRECTION ( 'NONE',  ( 0.000000000000000000, 1.000000000000000000, 0.000000000000000000 ) ) ;
#12921 = ORIENTED_EDGE ( 'NONE', *, *, #23862, .F. ) ;
#12922 = CARTESIAN_POINT ( 'NONE',  ( 44.06606138205700063, 40.39281886181299797, 82.55501292736983032 ) ) ;
#12923 = DIRECTION ( 'NONE',  ( 1.000000000000000000, 2.999999999999999839E-15, 0.000000000000000000 ) ) ;
#12924 = CARTESIAN_POINT ( 'NONE',  ( 40.33642880535521869, -13.30384086642190944, 69.98269868914866265 ) ) ;
#12925 = CIRCLE ( 'NONE', #13329, 0.7499999999999996669 ) ;
#12926 = CARTESIAN_POINT ( 'NONE',  ( 44.71606138205694947, 3.586515973360805187, -0.5067327973472466329 ) ) ;
#12927 = CARTESIAN_POINT ( 'NONE',  ( 36.80608444377001121, -21.31368208888610027, 70.35351908239857721 ) ) ;
#12928 = FACE_OUTER_BOUND ( 'NONE', #13130, .T. ) ;
#12929 = EDGE_CURVE ( 'NONE', #17722, #24841, #20334, .T. ) ;
#12930 = CIRCLE ( 'NONE', #21565, 0.9999999999999937828 ) ;
#12931 = LINE ( 'NONE', #12677, #22130 ) ;
#12932 = VERTEX_POINT ( 'NONE', #1416 ) ;
#12933 = CARTESIAN_POINT ( 'NONE',  ( 43.31606138205700063, -10.19550266980812658, 14.63954348514304904 ) ) ;
#12934 = FACE_OUTER_BOUND ( 'NONE', #7952, .T. ) ;
#12935 = CARTESIAN_POINT ( 'NONE',  ( 38.26194895904384907, -8.603840866421915479, 73.11602215082118050 ) ) ;
#12936 = DIRECTION ( 'NONE',  ( 1.000000000000000000, 0.000000000000000000, 0.000000000000000000 ) ) ;
#12937 = DIRECTION ( 'NONE',  ( 0.000000000000000000, 0.3299742535180969494, -0.9439899321577399638 ) ) ;
#12938 = CARTESIAN_POINT ( 'NONE',  ( 39.75915168707250302, -24.71368208888610241, 70.26145752964249880 ) ) ;
#12939 = CARTESIAN_POINT ( 'NONE',  ( 36.31606138205700773, -21.39087554181787354, 28.82307548518891238 ) ) ;
#12940 = AXIS2_PLACEMENT_3D ( 'NONE', #12421, #16260, #14219 ) ;
#12941 = AXIS2_PLACEMENT_3D ( 'NONE', #8079, #4083, #13749 ) ;
#12942 = CARTESIAN_POINT ( 'NONE',  ( 36.80608444377001831, -24.30384086642191832, 72.40698646996133903 ) ) ;
#12943 = CARTESIAN_POINT ( 'NONE',  ( 37.79585267494195477, -22.16015963634850650, 75.80517796092046012 ) ) ;
#12944 = VECTOR ( 'NONE', #13340, 1000.000000000000114 ) ;
#12945 = CARTESIAN_POINT ( 'NONE',  ( 36.87297107704152666, -27.71368208888610241, 72.49904802271738902 ) ) ;
#12946 = ORIENTED_EDGE ( 'NONE', *, *, #9081, .T. ) ;
#12947 = ORIENTED_EDGE ( 'NONE', *, *, #4697, .F. ) ;
#12948 = CARTESIAN_POINT ( 'NONE',  ( 31.81606138205700418, -36.10876147765401356, 70.30501292737011454 ) ) ;
#12949 = CARTESIAN_POINT ( 'NONE',  ( 44.81606138205700063, -26.97987052895604876, 80.55501292737007191 ) ) ;
#12950 = CARTESIAN_POINT ( 'NONE',  ( 37.69225076346193504, 0.1863179111138979493, 72.33091598616827866 ) ) ;
#12951 = CARTESIAN_POINT ( 'NONE',  ( 37.89291511884476904, -1.113682088886101207, 70.26206559358664094 ) ) ;
#12952 = ORIENTED_EDGE ( 'NONE', *, *, #25366, .F. ) ;
#12953 = VERTEX_POINT ( 'NONE', #17017 ) ;
#12954 = CARTESIAN_POINT ( 'NONE',  ( 35.31606138205700773, 7.187001342539796944, 66.09667597968754649 ) ) ;
#12955 = LINE ( 'NONE', #14741, #5041 ) ;
#12956 = VERTEX_POINT ( 'NONE', #15070 ) ;
#12957 = SURFACE_SIDE_STYLE ('',( #16418 ) ) ;
#12958 = CARTESIAN_POINT ( 'NONE',  ( 39.98359781491296161, -3.203840866421912903, 70.89533451361947414 ) ) ;
#12959 = EDGE_CURVE ( 'NONE', #15432, #14470, #9300, .T. ) ;
#12960 = EDGE_CURVE ( 'NONE', #16840, #13333, #25225, .T. ) ;
#12961 = CARTESIAN_POINT ( 'NONE',  ( 43.81606138205700063, -37.34243788671330577, 70.80615726751818784 ) ) ;
#12962 = ADVANCED_FACE ( 'NONE', ( #5285 ), #1287, .T. ) ;
#12963 = DIRECTION ( 'NONE',  ( 0.000000000000000000, -1.000000000000000000, 2.643388153869420804E-15 ) ) ;
#12964 = ORIENTED_EDGE ( 'NONE', *, *, #1215, .T. ) ;
#12965 = ORIENTED_EDGE ( 'NONE', *, *, #18708, .T. ) ;
#12966 = ORIENTED_EDGE ( 'NONE', *, *, #1226, .T. ) ;
#12967 = CARTESIAN_POINT ( 'NONE',  ( 43.81606138205700063, 3.172506336381830661, 12.50058896911730066 ) ) ;
#12968 = CARTESIAN_POINT ( 'NONE',  ( 36.49096545463212493, -1.513682088886105559, 71.43714994484035685 ) ) ;
#12969 = B_SPLINE_CURVE_WITH_KNOTS ( 'NONE', 3,
 ( #16886, #24966, #13024, #5169, #19317, #5544, #5662, #17393, #25226, #15193, #7610, #19440, #23049, #1786, #21133, #3476 ),
 .UNSPECIFIED., .F., .F.,
 ( 4, 2, 2, 2, 2, 2, 2, 4 ),
 ( 0.000000000000000000, 0.1250000000000009992, 0.2500000000000004441, 0.3749999999999998890, 0.4999999999999991118, 0.6250000000000002220, 0.7500000000000011102, 1.000000000000000000 ),
 .UNSPECIFIED. ) ;
#12970 = CARTESIAN_POINT ( 'NONE',  ( 36.81465384343994884, 41.90149715599300606, 79.87823623207322044 ) ) ;
#12971 = PLANE ( 'NONE',  #16156 ) ;
#12972 = ORIENTED_EDGE ( 'NONE', *, *, #17591, .F. ) ;
#12973 = CYLINDRICAL_SURFACE ( 'NONE', #20928, 1.750000000000001554 ) ;
#12974 = EDGE_CURVE ( 'NONE', #24574, #1612, #17140, .T. ) ;
#12975 = CARTESIAN_POINT ( 'NONE',  ( 41.81606138205700063, -2.300394311618905174, 46.75701924734788406 ) ) ;
#12976 = LINE ( 'NONE', #20824, #15203 ) ;
#12977 = CARTESIAN_POINT ( 'NONE',  ( 42.68042513965293949, 2.191238522347013440, 73.80501292737000085 ) ) ;
#12978 =( NAMED_UNIT ( * ) SI_UNIT ( $, .STERADIAN. ) SOLID_ANGLE_UNIT ( ) );
#12979 = CARTESIAN_POINT ( 'NONE',  ( 33.31606138205700773, 3.296535697557910538, 65.33616386252352015 ) ) ;
#12980 = VERTEX_POINT ( 'NONE', #3214 ) ;
#12981 = EDGE_LOOP ( 'NONE', ( #17358, #4029, #13723, #14391, #11497, #2910, #22080, #7434, #3915, #5309, #20836, #10173 ) ) ;
#12982 = VECTOR ( 'NONE', #23704, 1000.000000000000000 ) ;
#12983 = LINE ( 'NONE', #5121, #24756 ) ;
#12984 = DIRECTION ( 'NONE',  ( 0.000000000000000000, 3.469446951953613400E-15, 1.000000000000000000 ) ) ;
#12985 = CARTESIAN_POINT ( 'NONE',  ( 38.37017380507020192, -18.01368208888610312, 72.51602215082118619 ) ) ;
#12986 = VERTEX_POINT ( 'NONE', #11602 ) ;
#12987 = ORIENTED_EDGE ( 'NONE', *, *, #14602, .T. ) ;
#12988 = CARTESIAN_POINT ( 'NONE',  ( 35.64099152588523367, -8.607181138186998481, 88.30501292736998664 ) ) ;
#12989 = CARTESIAN_POINT ( 'NONE',  ( 36.80608444377001121, 0.6863179111138983934, 70.35351908239860563 ) ) ;
#12990 = CARTESIAN_POINT ( 'NONE',  ( 39.75915168707251723, -22.90384086642190908, 72.49904802271738902 ) ) ;
#12991 = FACE_OUTER_BOUND ( 'NONE', #8606, .T. ) ;
#12992 = CARTESIAN_POINT ( 'NONE',  ( 36.07789103942398867, -7.413682088886105248, 70.70992431699450265 ) ) ;
#12993 = LINE ( 'NONE', #16849, #8217 ) ;
#12994 = ORIENTED_EDGE ( 'NONE', *, *, #16974, .T. ) ;
#12995 = DIRECTION ( 'NONE',  ( 0.000000000000000000, -0.8213699656732942334, 0.5703958094953462954 ) ) ;
#12996 = CARTESIAN_POINT ( 'NONE',  ( 43.81606138205700063, 36.92314894770294131, 81.37823623207324886 ) ) ;
#12997 = LINE ( 'NONE', #22894, #7100 ) ;
#12998 = CARTESIAN_POINT ( 'NONE',  ( 33.31606138205700773, -19.92642959707779227, 24.72592537066031682 ) ) ;
#12999 = FACE_OUTER_BOUND ( 'NONE', #11652, .T. ) ;
#13000 = EDGE_CURVE ( 'NONE', #10641, #12591, #15325, .T. ) ;
#13001 = DIRECTION ( 'NONE',  ( 1.000000000000000000, 2.999999999999999839E-15, 0.000000000000000000 ) ) ;
#13002 = VERTEX_POINT ( 'NONE', #3596 ) ;
#13003 = CYLINDRICAL_SURFACE ( 'NONE', #12754, 1.000000000000000888 ) ;
#13004 = CARTESIAN_POINT ( 'NONE',  ( 36.56606138205700063, 6.004618353093779781, 2.291321535809666354 ) ) ;
#13005 = ORIENTED_EDGE ( 'NONE', *, *, #13503, .T. ) ;
#13006 = ORIENTED_EDGE ( 'NONE', *, *, #12429, .T. ) ;
#13007 = CARTESIAN_POINT ( 'NONE',  ( 40.55423172469004101, -17.20384086642191335, 70.70992431699450265 ) ) ;
#13008 = CARTESIAN_POINT ( 'NONE',  ( 36.87297107704152666, -19.71368208888610951, 72.49904802271740323 ) ) ;
#13009 = CARTESIAN_POINT ( 'NONE',  ( 36.31606138205702194, -19.40517585842703241, 23.66972737280834238 ) ) ;
#13010 = EDGE_CURVE ( 'NONE', #18120, #5267, #9643, .T. ) ;
#13011 = VERTEX_POINT ( 'NONE', #11477 ) ;
#13012 = LINE ( 'NONE', #14553, #21207 ) ;
#13013 = DIRECTION ( 'NONE',  ( -2.417197558325568929E-15, 0.6529557272876933549, 0.7573960774932753104 ) ) ;
#13014 = CARTESIAN_POINT ( 'NONE',  ( 39.64521430340304420, -28.81368208888610383, 69.45876917294174291 ) ) ;
#13015 = EDGE_LOOP ( 'NONE', ( #5099, #3924 ) ) ;
#13016 = EDGE_CURVE ( 'NONE', #4112, #14925, #16200, .T. ) ;
#13017 = FACE_BOUND ( 'NONE', #12577, .T. ) ;
#13018 = CARTESIAN_POINT ( 'NONE',  ( 39.38009889167650357, -4.213682088886106847, 72.75271321436733274 ) ) ;
#13019 = DIRECTION ( 'NONE',  ( 1.000000000000000000, 8.911169920151748851E-16, 3.114923731923493702E-16 ) ) ;
#13020 = ORIENTED_EDGE ( 'NONE', *, *, #9585, .T. ) ;
#13021 = CARTESIAN_POINT ( 'NONE',  ( 36.49096545463212493, -19.51368208888610312, 71.43714994484034264 ) ) ;
#13022 = CARTESIAN_POINT ( 'NONE',  ( 43.31606138205700063, -26.06829118875199214, 77.52306850662461102 ) ) ;
#13023 = EDGE_CURVE ( 'NONE', #15007, #13507, #11224, .T. ) ;
#13024 = CARTESIAN_POINT ( 'NONE',  ( 38.05217264712879199, -5.217354499694973669, 83.30503613834979149 ) ) ;
#13025 = CARTESIAN_POINT ( 'NONE',  ( 37.25260217561390874, -20.00384086642191406, 70.97781676520601479 ) ) ;
#13026 = CARTESIAN_POINT ( 'NONE',  ( 38.26194895904383486, -3.013682088886100008, 69.64448340153879258 ) ) ;
#13027 = ORIENTED_EDGE ( 'NONE', *, *, #17919, .T. ) ;
#13028 = FACE_OUTER_BOUND ( 'NONE', #15784, .T. ) ;
#13029 = VERTEX_POINT ( 'NONE', #18948 ) ;
#13030 = CARTESIAN_POINT ( 'NONE',  ( 39.38009889167648936, -5.403840866421906419, 70.00779233799264034 ) ) ;
#13031 = DIRECTION ( 'NONE',  ( -9.027796614315171564E-31, -1.000000000000000000, -1.163336342344335610E-15 ) ) ;
#13032 = CARTESIAN_POINT ( 'NONE',  ( 36.64852494920107517, 0.5863179111138955291, 70.89533451361948835 ) ) ;
#13033 = VERTEX_POINT ( 'NONE', #24850 ) ;
#13034 = CARTESIAN_POINT ( 'NONE',  ( 40.55423172469004811, -8.413682088886105248, 72.05058123536544201 ) ) ;
#13035 = VERTEX_POINT ( 'NONE', #7224 ) ;
#13036 = DIRECTION ( 'NONE',  ( 0.000000000000000000, -1.000000000000000000, 2.999999999999999839E-15 ) ) ;
#13037 = CARTESIAN_POINT ( 'NONE',  ( 38.37017380507018771, -11.60384086642191015, 70.24448340153877268 ) ) ;
#13038 = EDGE_CURVE ( 'NONE', #11458, #15185, #12969, .T. ) ;
#13039 = DIRECTION ( 'NONE',  ( 0.000000000000000000, 1.000000000000000000, 0.000000000000000000 ) ) ;
#13040 = ADVANCED_FACE ( 'NONE', ( #11351 ), #15954, .T. ) ;
#13041 = ORIENTED_EDGE ( 'NONE', *, *, #19626, .T. ) ;
#13042 = DIRECTION ( 'NONE',  ( -0.000000000000000000, -0.7540134720837717852, -0.6568589528324747517 ) ) ;
#13043 = LINE ( 'NONE', #24356, #16187 ) ;
#13044 = CARTESIAN_POINT ( 'NONE',  ( 37.50301148336529877, -18.50384086642192116, 73.69843995877327814 ) ) ;
#13045 = EDGE_CURVE ( 'NONE', #20035, #23539, #12108, .T. ) ;
#13046 = EDGE_CURVE ( 'NONE', #8243, #4589, #11703, .T. ) ;
#13047 = EDGE_CURVE ( 'NONE', #11457, #16794, #2295, .T. ) ;
#13048 = CARTESIAN_POINT ( 'NONE',  ( 36.31606138205700063, -20.22127907754186893, 75.50705395623725735 ) ) ;
#13049 =( NAMED_UNIT ( * ) PLANE_ANGLE_UNIT ( ) SI_UNIT ( $, .RADIAN. ) );
#13050 = CARTESIAN_POINT ( 'NONE',  ( 36.49096545463212493, -21.51368208888609956, 71.43714994484034264 ) ) ;
#13051 = PLANE ( 'NONE',  #18405 ) ;
#13052 = DIRECTION ( 'NONE',  ( 9.251858538542962756E-15, 1.000000000000000000, 0.000000000000000000 ) ) ;
#13053 = VERTEX_POINT ( 'NONE', #21510 ) ;
#13054 = LINE ( 'NONE', #22835, #4686 ) ;
#13055 = FACE_OUTER_BOUND ( 'NONE', #14998, .T. ) ;
#13056 = EDGE_CURVE ( 'NONE', #16916, #9369, #9241, .T. ) ;
#13057 = CARTESIAN_POINT ( 'NONE',  ( 37.69796330110505522, -8.503840866421915834, 73.09843995877331224 ) ) ;
#13058 = VECTOR ( 'NONE', #11888, 1000.000000000000227 ) ;
#13060 = ADVANCED_FACE ( 'NONE', ( #15575, #21892 ), #15833, .F. ) ;
#13059 = PRODUCT_CONTEXT ( 'NONE', #4370, 'mechanical' ) ;
#13061 = CARTESIAN_POINT ( 'NONE',  ( 33.22724336997212902, 3.110414846328807936, 6.134845797670998913 ) ) ;
#13062 = CARTESIAN_POINT ( 'NONE',  ( 36.80608444377001121, -27.31368208888610383, 70.35351908239857721 ) ) ;
#13063 = AXIS2_PLACEMENT_3D ( 'NONE', #1814, #5690, #21162 ) ;
#13064 = AXIS2_PLACEMENT_3D ( 'NONE', #16927, #18857, #20404 ) ;
#13065 = CARTESIAN_POINT ( 'NONE',  ( 34.66606138205693810, 6.105630034208187062, 5.871938670042847974 ) ) ;
#13066 = CARTESIAN_POINT ( 'NONE',  ( 36.87297107704149823, -21.90384086642189843, 70.26145752964252722 ) ) ;
#13067 = CARTESIAN_POINT ( 'NONE',  ( 37.67019652925851148, -5.306778407178573964, 83.30463327861060918 ) ) ;
#13068 = CARTESIAN_POINT ( 'NONE',  ( 36.87297107704152666, -25.71368208888609885, 72.49904802271738902 ) ) ;
#13069 = ORIENTED_EDGE ( 'NONE', *, *, #21377, .T. ) ;
#13070 = CARTESIAN_POINT ( 'NONE',  ( 38.26194895904384197, 1.396159133578080080, 73.71602215082117482 ) ) ;
#13071 = EDGE_LOOP ( 'NONE', ( #19054, #5186, #6470, #12576 ) ) ;
#13072 = DIRECTION ( 'NONE',  ( 0.000000000000000000, 0.6568589528324746407, -0.7540134720837717852 ) ) ;
#13073 = PLANE ( 'NONE',  #516 ) ;
#13074 = CARTESIAN_POINT ( 'NONE',  ( 38.73920764526925353, -2.113682088886101873, 72.49843995877331793 ) ) ;
#13075 = EDGE_LOOP ( 'NONE', ( #42, #20330, #1067, #8804 ) ) ;
#13076 = ORIENTED_EDGE ( 'NONE', *, *, #10328, .F. ) ;
#13077 = LINE ( 'NONE', #3270, #2641 ) ;
#13078 = CARTESIAN_POINT ( 'NONE',  ( 43.31606138205700063, 4.103895195095678794, 6.341006091748962348 ) ) ;
#13079 = ORIENTED_EDGE ( 'NONE', *, *, #24272, .T. ) ;
#13080 = CARTESIAN_POINT ( 'NONE',  ( 38.26194895904384907, -6.603840866421916367, 73.11602215082118050 ) ) ;
#13081 = CLOSED_SHELL ( 'NONE', ( #23615, #21165, #258, #16386, #3111, #25118, #6214, #24284, #12395, #16817, #23650, #21617, #25042, #11856, #9102, #19692, #10056, #1466, #8899, #13393, #106, #16787, #7770, #4391 ) ) ;
#13082 = CIRCLE ( 'NONE', #19652, 1.000000000000000888 ) ;
#13083 = VECTOR ( 'NONE', #7682, 1000.000000000000000 ) ;
#13084 = LINE ( 'NONE', #13833, #1813 ) ;
#13085 = CARTESIAN_POINT ( 'NONE',  ( 38.14273442609844977, 40.69123852234599781, 70.32014858831708182 ) ) ;
#13086 = VERTEX_POINT ( 'NONE', #25351 ) ;
#13087 = EDGE_LOOP ( 'NONE', ( #20546, #23661, #659, #22811 ) ) ;
#13088 = CARTESIAN_POINT ( 'NONE',  ( 32.56606138205700773, 41.63025572888945192, 83.79244979444629848 ) ) ;
#13089 = CARTESIAN_POINT ( 'NONE',  ( 40.14115730948191185, -2.513682088886103116, 71.32335560751961623 ) ) ;
#13090 = CARTESIAN_POINT ( 'NONE',  ( 39.29254315202757653, -26.80384086642191477, 72.81632618279320468 ) ) ;
#13091 = SHAPE_REPRESENTATION_RELATIONSHIP ( 'NONE' , 'NONE' ,  #8505, #20587 ) ;
#13092 = LINE ( 'NONE', #20944, #21519 ) ;
#13093 = ORIENTED_EDGE ( 'NONE', *, *, #1022, .T. ) ;
#13094 = CARTESIAN_POINT ( 'NONE',  ( 32.31606138205700063, 9.733755362416909307, 68.18201966341686671 ) ) ;
#13095 = DIRECTION ( 'NONE',  ( 0.000000000000000000, -1.000000000000000000, 2.999999999999999839E-15 ) ) ;
#13096 = CIRCLE ( 'NONE', #1964, 0.5000000000000019984 ) ;
#13097 = EDGE_CURVE ( 'NONE', #10140, #4783, #17852, .T. ) ;
#13098 =( BOUNDED_CURVE ( )  B_SPLINE_CURVE ( 3, ( #19761, #2102, #17844, #4180 ),
 .UNSPECIFIED., .F., .T. ) 
 B_SPLINE_CURVE_WITH_KNOTS ( ( 4, 4 ),
 ( 1.570796326794895004, 3.141592653589795336 ),
 .UNSPECIFIED. ) 
 CURVE ( )  GEOMETRIC_REPRESENTATION_ITEM ( )  RATIONAL_B_SPLINE_CURVE ( ( 1.000000000000000000, 0.8047378541243649375, 0.8047378541243649375, 1.000000000000000000 ) ) 
 REPRESENTATION_ITEM ( '' )  );
#13099 = DIRECTION ( 'NONE',  ( -1.000000000000000000, 0.000000000000000000, 0.000000000000000000 ) ) ;
#13100 = DIRECTION ( 'NONE',  ( -4.256992727861094749E-32, 1.000000000000000000, -3.115648231731786715E-15 ) ) ;
#13101 =( NAMED_UNIT ( * ) SI_UNIT ( $, .STERADIAN. ) SOLID_ANGLE_UNIT ( ) );
#13102 = EDGE_CURVE ( 'NONE', #8461, #4335, #12122, .T. ) ;
#13103 = AXIS2_PLACEMENT_3D ( 'NONE', #5598, #25408, #17579 ) ;
#13104 = VECTOR ( 'NONE', #7163, 1000.000000000000227 ) ;
#13105 = PRODUCT_RELATED_PRODUCT_CATEGORY ( 'part', '', ( #19806 ) ) ;
#13106 = LINE ( 'NONE', #972, #8695 ) ;
#13107 = ORIENTED_EDGE ( 'NONE', *, *, #261, .T. ) ;
#13108 = VERTEX_POINT ( 'NONE', #21635 ) ;
#13109 = CARTESIAN_POINT ( 'NONE',  ( 47.84183937708599643, -34.55876147765400219, 70.30501292737000085 ) ) ;
#13110 = DIRECTION ( 'NONE',  ( 1.022195611122249672E-16, -0.1771812806364704007, -0.9841782327363373106 ) ) ;
#13111 = CARTESIAN_POINT ( 'NONE',  ( 38.00113996487114321, -19.91368208888610170, 72.53360434286904024 ) ) ;
#13112 = ORIENTED_EDGE ( 'NONE', *, *, #23432, .F. ) ;
#13113 = EDGE_LOOP ( 'NONE', ( #10032, #5175, #6678, #10120 ) ) ;
#13114 = DIRECTION ( 'NONE',  ( 1.734723475976804876E-16, 2.999999999999999839E-15, 1.000000000000000000 ) ) ;
#13115 = DIRECTION ( 'NONE',  ( 0.000000000000000000, 0.000000000000000000, -1.000000000000000000 ) ) ;
#13116 = CARTESIAN_POINT ( 'NONE',  ( 38.82593461698265003, -24.70384086642191690, 73.13360434286902034 ) ) ;
#13117 = DIRECTION ( 'NONE',  ( 1.000000000000000000, 0.000000000000000000, 0.000000000000000000 ) ) ;
#13118 = CARTESIAN_POINT ( 'NONE',  ( 40.55423172469004811, -4.413682088886105248, 72.05058123536544201 ) ) ;
#13119 = ORIENTED_EDGE ( 'NONE', *, *, #3014, .F. ) ;
#13120 = AXIS2_PLACEMENT_3D ( 'NONE', #6649, #2896, #4843 ) ;
#13121 = DIRECTION ( 'NONE',  ( 0.000000000000000000, 0.5706330172266920187, -0.8212051873014210024 ) ) ;
#13122 = LINE ( 'NONE', #24816, #15107 ) ;
#13123 = CARTESIAN_POINT ( 'NONE',  ( 43.31606138205700063, 3.099306811489555891, 65.29760936252343129 ) ) ;
#13124 = CARTESIAN_POINT ( 'NONE',  ( 39.20459794252392527, -5.397949909403978452, 82.80325005500586144 ) ) ;
#13125 = DIRECTION ( 'NONE',  ( 0.000000000000000000, 1.000000000000000000, 0.000000000000000000 ) ) ;
#13126 = EDGE_CURVE ( 'NONE', #19881, #59, #9588, .T. ) ;
#13127 =( GEOMETRIC_REPRESENTATION_CONTEXT ( 3 ) GLOBAL_UNCERTAINTY_ASSIGNED_CONTEXT ( ( #8446 ) ) GLOBAL_UNIT_ASSIGNED_CONTEXT ( ( #22278, #2687, #18549 ) ) REPRESENTATION_CONTEXT ( 'NONE', 'WORKASPACE' ) );
#13128 = CARTESIAN_POINT ( 'NONE',  ( 43.31606138205700063, -35.70002751211045933, 71.94742330197156832 ) ) ;
#13129 = ADVANCED_FACE ( 'NONE', ( #10170 ), #18037, .F. ) ;
#13130 = EDGE_LOOP ( 'NONE', ( #5677, #17569, #847, #6682 ) ) ;
#13131 = DIRECTION ( 'NONE',  ( 1.000000000000000275E-15, -0.9439899321577401858, -0.3299742535180970604 ) ) ;
#13132 = FACE_OUTER_BOUND ( 'NONE', #20973, .T. ) ;
#13133 = EDGE_LOOP ( 'NONE', ( #25269, #8323, #21874, #14956 ) ) ;
#13134 = VERTEX_POINT ( 'NONE', #23560 ) ;
#13135 = CARTESIAN_POINT ( 'NONE',  ( 39.64521430340305841, -12.80384086642191832, 73.30173637941818754 ) ) ;
#13136 = VECTOR ( 'NONE', #1978, 1000.000000000000114 ) ;
#13137 = DIRECTION ( 'NONE',  ( 1.000000000000000000, 0.000000000000000000, -0.000000000000000000 ) ) ;
#13138 = CARTESIAN_POINT ( 'NONE',  ( 38.26194895904383486, -21.01368208888610312, 69.64448340153877837 ) ) ;
#13139 = VECTOR ( 'NONE', #6180, 1000.000000000000000 ) ;
#13140 = VERTEX_POINT ( 'NONE', #8240 ) ;
#13141 = DIRECTION ( 'NONE',  ( -1.000000000000000000, 0.000000000000000000, 0.000000000000000000 ) ) ;
#13142 = LINE ( 'NONE', #9289, #5516 ) ;
#13143 = EDGE_CURVE ( 'NONE', #19656, #16125, #7164, .T. ) ;
#13144 = CARTESIAN_POINT ( 'NONE',  ( 40.26954217208371034, -20.71368208888610596, 69.89063713639258424 ) ) ;
#13145 = VERTEX_POINT ( 'NONE', #9796 ) ;
#13146 = AXIS2_PLACEMENT_3D ( 'NONE', #18293, #16331, #14415 ) ;
#13147 = LINE ( 'NONE', #16611, #11070 ) ;
#13148 = CARTESIAN_POINT ( 'NONE',  ( 40.14115730948191185, -0.5136820888861047818, 71.32335560751961623 ) ) ;
#13149 = CARTESIAN_POINT ( 'NONE',  ( 36.81465384343994884, 41.90149715599300606, 79.37823623207322044 ) ) ;
#13150 = CARTESIAN_POINT ( 'NONE',  ( 39.75915168707250302, -14.71368208888610063, 70.26145752964252722 ) ) ;
#13151 = AXIS2_PLACEMENT_3D ( 'NONE', #2704, #16365, #22426 ) ;
#13152 = DIRECTION ( 'NONE',  ( 0.000000000000000000, 1.000000000000000000, -2.999999999999999839E-15 ) ) ;
#13153 = DIRECTION ( 'NONE',  ( 2.312964634635742661E-15, -0.4425581086832398037, 0.8967398287344628960 ) ) ;
#13154 = AXIS2_PLACEMENT_3D ( 'NONE', #4856, #3169, #24917 ) ;
#13155 = CARTESIAN_POINT ( 'NONE',  ( 39.24876120206129571, -16.90384086642190553, 72.12822762946747446 ) ) ;
#13156 = CARTESIAN_POINT ( 'NONE',  ( 39.38009889167650357, -8.213682088886105959, 72.75271321436733274 ) ) ;
#13157 = VERTEX_POINT ( 'NONE', #23687 ) ;
#13158 = DIRECTION ( 'NONE',  ( 1.218693434051482139E-16, -0.4425581086832393041, 0.8967398287344630070 ) ) ;
#13159 = ORIENTED_EDGE ( 'NONE', *, *, #12418, .T. ) ;
#13160 = EDGE_LOOP ( 'NONE', ( #2481, #19378, #20799, #15023 ) ) ;
#13161 = AXIS2_PLACEMENT_3D ( 'NONE', #13884, #6027, #11971 ) ;
#13162 = CARTESIAN_POINT ( 'NONE',  ( 39.29254315202757653, -4.803840866421913880, 72.81632618279323310 ) ) ;
#13163 = DIRECTION ( 'NONE',  ( 1.000000000000000000, 1.000000000000000078E-15, 0.000000000000000000 ) ) ;
#13164 = CARTESIAN_POINT ( 'NONE',  ( 38.37017380507020192, -2.013682088886109334, 73.11602215082118050 ) ) ;
#13165 = VERTEX_POINT ( 'NONE', #17783 ) ;
#13166 = CARTESIAN_POINT ( 'NONE',  ( 37.50301148336529167, -7.113682088886103649, 69.06206559358666652 ) ) ;
#13167 = EDGE_LOOP ( 'NONE', ( #14246, #6640, #20536, #4103 ) ) ;
#13168 = FACE_OUTER_BOUND ( 'NONE', #3098, .T. ) ;
#13169 = CARTESIAN_POINT ( 'NONE',  ( 37.12184278917507640, -8.103840866421910150, 71.32335560751961623 ) ) ;
#13170 = VECTOR ( 'NONE', #20729, 1000.000000000000000 ) ;
#13171 = FACE_OUTER_BOUND ( 'NONE', #582, .T. ) ;
#13172 = EDGE_LOOP ( 'NONE', ( #13112, #21475, #2387, #19418 ) ) ;
#13173 = DIRECTION ( 'NONE',  ( 1.000000000000000000, 1.734723475976804876E-16, -1.734723475976814737E-16 ) ) ;
#13174 = DIRECTION ( 'NONE',  ( -1.000000000000000000, 0.000000000000000000, 0.000000000000000000 ) ) ;
#13175 = EDGE_CURVE ( 'NONE', #2290, #6422, #110, .T. ) ;
#13176 = CARTESIAN_POINT ( 'NONE',  ( 38.26194895904384197, -16.60384086642191548, 73.71602215082113219 ) ) ;
#13177 = VECTOR ( 'NONE', #8782, 1000.000000000000000 ) ;
#13178 = CARTESIAN_POINT ( 'NONE',  ( 36.57656417722905928, -21.21691551846920731, 75.35497464634362075 ) ) ;
#13179 = CARTESIAN_POINT ( 'NONE',  ( 39.98359781491296161, -22.41368208888610525, 71.86517103874047052 ) ) ;
#13180 = FACE_OUTER_BOUND ( 'NONE', #18096, .T. ) ;
#13181 = AXIS2_PLACEMENT_3D ( 'NONE', #7779, #2087, #13573 ) ;
#13182 = CARTESIAN_POINT ( 'NONE',  ( 45.81606138205695089, 1.773964314019564448, -3.427682652428129195 ) ) ;
#13183 = AXIS2_PLACEMENT_3D ( 'NONE', #23439, #25095, #15838 ) ;
#13184 = VERTEX_POINT ( 'NONE', #5797 ) ;
#13185 = FACE_OUTER_BOUND ( 'NONE', #22784, .T. ) ;
#13186 = DIRECTION ( 'NONE',  ( -1.445602896647339903E-16, 1.000000000000000000, -2.999999999999999839E-15 ) ) ;
#13187 = CARTESIAN_POINT ( 'NONE',  ( 36.80608444377002542, -6.303840866421914768, 72.40698646996135324 ) ) ;
#13188 = CARTESIAN_POINT ( 'NONE',  ( 33.33836326447716658, 3.869514117107255569, 6.310928887378282504 ) ) ;
#13189 = EDGE_CURVE ( 'NONE', #17064, #17020, #11863, .T. ) ;
#13190 = CARTESIAN_POINT ( 'NONE',  ( 36.49096545463212493, -23.51368208888609601, 71.43714994484030001 ) ) ;
#13191 = ADVANCED_FACE ( 'NONE', ( #7995 ), #15708, .F. ) ;
#13192 = LINE ( 'NONE', #23085, #20945 ) ;
#13193 = EDGE_CURVE ( 'NONE', #2757, #24470, #17040, .T. ) ;
#13194 = ADVANCED_FACE ( 'NONE', ( #17527 ), #486, .F. ) ;
#13195 = CARTESIAN_POINT ( 'NONE',  ( 39.38009889167648936, -23.40384086642190908, 70.00779233799262613 ) ) ;
#13196 = EDGE_CURVE ( 'NONE', #59, #6765, #8979, .T. ) ;
#13197 = CARTESIAN_POINT ( 'NONE',  ( 44.31606138205700063, -20.93319939328399926, 43.78741072286599945 ) ) ;
#13198 = CARTESIAN_POINT ( 'NONE',  ( 37.69796330110504101, -17.11368208888610098, 69.66206559358661821 ) ) ;
#13199 = EDGE_LOOP ( 'NONE', ( #22865, #24018, #14044, #11396 ) ) ;
#13200 = CARTESIAN_POINT ( 'NONE',  ( 40.55423172469004101, 0.7961591335780838774, 70.70992431699450265 ) ) ;
#13201 = VERTEX_POINT ( 'NONE', #15018 ) ;
#13202 = LINE ( 'NONE', #12948, #23016 ) ;
#13203 = CYLINDRICAL_SURFACE ( 'NONE', #938, 1.750000000000001554 ) ;
#13204 = VECTOR ( 'NONE', #14921, 1000.000000000000000 ) ;
#13205 = CARTESIAN_POINT ( 'NONE',  ( 37.60469502381300799, -24.40384086642190908, 72.26730301774232146 ) ) ;
#13206 = ORIENTED_EDGE ( 'NONE', *, *, #23492, .T. ) ;
#13207 = VERTEX_POINT ( 'NONE', #9116 ) ;
#13208 = CARTESIAN_POINT ( 'NONE',  ( 31.81606138205700418, 38.19123852234598360, 71.05501292736988717 ) ) ;
#13209 = CARTESIAN_POINT ( 'NONE',  ( 29.81606138205696865, -3.028410647649181442, 0.3252050635115383281 ) ) ;
#13210 = ORIENTED_EDGE ( 'NONE', *, *, #3112, .F. ) ;
#13211 = EDGE_CURVE ( 'NONE', #8863, #2531, #22745, .T. ) ;
#13212 = FACE_OUTER_BOUND ( 'NONE', #14857, .T. ) ;
#13213 = CARTESIAN_POINT ( 'NONE',  ( 38.26194895904384907, -2.603840866421916367, 73.11602215082118050 ) ) ;
#13214 = EDGE_CURVE ( 'NONE', #21810, #14863, #1399, .T. ) ;
#13215 = LINE ( 'NONE', #22608, #12944 ) ;
#13216 = B_SPLINE_SURFACE_WITH_KNOTS ( 'NONE', 1, 3, ( 
 ( #11167, #11303, #1855, #1480 ),
 ( #13230, #7424, #23369, #7293 ) ),
 .UNSPECIFIED., .F., .F., .F.,
 ( 2, 2 ),
 ( 4, 4 ),
 ( 0.000000000000000000, 1.000000000000000000 ),
 ( 0.000000000000000000, 1.000000000000000000 ),
 .UNSPECIFIED. ) ;
#13217 = DIRECTION ( 'NONE',  ( -1.000000000000000000, -1.052872940142565459E-15, -1.848188032574765003E-17 ) ) ;
#13218 = ORIENTED_EDGE ( 'NONE', *, *, #574, .F. ) ;
#13219 = ORIENTED_EDGE ( 'NONE', *, *, #21219, .T. ) ;
#13220 = CARTESIAN_POINT ( 'NONE',  ( 40.64099152588522657, 1.392818861812999964, 83.30501292736997243 ) ) ;
#13221 = VECTOR ( 'NONE', #18931, 1000.000000000000000 ) ;
#13222 = CARTESIAN_POINT ( 'NONE',  ( 39.82603832034401847, -0.3136820888861094336, 72.40698646996133903 ) ) ;
#13223 = ADVANCED_FACE ( 'NONE', ( #2548 ), #11166, .T. ) ;
#13224 = CARTESIAN_POINT ( 'NONE',  ( 39.95015449827720744, -27.00384086642191050, 71.96809898377885872 ) ) ;
#13225 =( LENGTH_UNIT ( ) NAMED_UNIT ( * ) SI_UNIT ( .MILLI., .METRE. ) );
#13226 = LINE ( 'NONE', #5731, #20696 ) ;
#13227 = AXIS2_PLACEMENT_3D ( 'NONE', #840, #5118, #14517 ) ;
#13228 = ORIENTED_EDGE ( 'NONE', *, *, #5627, .T. ) ;
#13229 = CYLINDRICAL_SURFACE ( 'NONE', #14737, 0.7500000000000006661 ) ;
#13230 = CARTESIAN_POINT ( 'NONE',  ( 43.31606138205700063, -33.60910547091194900, 60.61426200347987248 ) ) ;
#13231 = CARTESIAN_POINT ( 'NONE',  ( 44.71606138205697789, -5.918777154956154085, -5.916875169744970187 ) ) ;
#13232 =( LENGTH_UNIT ( ) NAMED_UNIT ( * ) SI_UNIT ( .MILLI., .METRE. ) );
#13233 = ORIENTED_EDGE ( 'NONE', *, *, #15467, .F. ) ;
#13234 = DIRECTION ( 'NONE',  ( 1.734723475976804876E-16, 3.469446951953610245E-15, 1.000000000000000000 ) ) ;
#13235 = ORIENTED_EDGE ( 'NONE', *, *, #1042, .F. ) ;
#13236 = ORIENTED_EDGE ( 'NONE', *, *, #25171, .T. ) ;
#13237 = CARTESIAN_POINT ( 'NONE',  ( 32.81606138205700773, 28.12806996228107437, 66.30501292736992980 ) ) ;
#13238 = DIRECTION ( 'NONE',  ( -0.3454074107579455100, -0.7706623348594876521, -0.5355121718713914403 ) ) ;
#13239 = CARTESIAN_POINT ( 'NONE',  ( 38.93987200065208754, -16.81368208888610383, 70.42958956619168021 ) ) ;
#13240 = ORIENTED_EDGE ( 'NONE', *, *, #12405, .F. ) ;
#13241 = EDGE_LOOP ( 'NONE', ( #25082, #415, #10391, #23792 ) ) ;
#13242 = FACE_OUTER_BOUND ( 'NONE', #11840, .T. ) ;
#13243 = EDGE_CURVE ( 'NONE', #23789, #9136, #4693, .T. ) ;
#13244 = CARTESIAN_POINT ( 'NONE',  ( 40.14115730948191185, 1.486317911113896884, 71.32335560751963044 ) ) ;
#13245 = CARTESIAN_POINT ( 'NONE',  ( 39.38009889167648936, -23.40384086642190908, 70.00779233799262613 ) ) ;
#13246 = AXIS2_PLACEMENT_3D ( 'NONE', #2507, #16682, #16543 ) ;
#13247 = CARTESIAN_POINT ( 'NONE',  ( 32.56606138205700773, -26.74044063519535186, 83.30501292737007191 ) ) ;
#13248 = AXIS2_PLACEMENT_3D ( 'NONE', #4525, #4647, #16237 ) ;
#13249 = CARTESIAN_POINT ( 'NONE',  ( 41.96606138205694236, 5.651448314156990449, 4.532640732625139002 ) ) ;
#13250 = EDGE_CURVE ( 'NONE', #16702, #1954, #1230, .T. ) ;
#13251 = FACE_OUTER_BOUND ( 'NONE', #10262, .T. ) ;
#13252 = CARTESIAN_POINT ( 'NONE',  ( 36.56606138205700063, 5.594015759443068170, 2.006005027196319901 ) ) ;
#13253 = CARTESIAN_POINT ( 'NONE',  ( 40.21566563214662438, -6.565621769560124221, 83.22218355014231861 ) ) ;
#13254 = DIRECTION ( 'NONE',  ( 1.000000000000000000, -0.000000000000000000, 0.000000000000000000 ) ) ;
#13255 = AXIS2_PLACEMENT_3D ( 'NONE', #9400, #23157, #13394 ) ;
#13256 = LINE ( 'NONE', #9654, #8200 ) ;
#13257 = ORIENTED_EDGE ( 'NONE', *, *, #6867, .T. ) ;
#13258 = FACE_OUTER_BOUND ( 'NONE', #22182, .T. ) ;
#13259 = CIRCLE ( 'NONE', #8739, 1.499999999999999778 ) ;
#13260 = LINE ( 'NONE', #21112, #23460 ) ;
#13261 = ORIENTED_EDGE ( 'NONE', *, *, #15385, .T. ) ;
#13262 = VERTEX_POINT ( 'NONE', #5114 ) ;
#13263 = CARTESIAN_POINT ( 'NONE',  ( 36.89935272106205133, -10.40384086642191797, 73.23812341099225875 ) ) ;
#13264 = CARTESIAN_POINT ( 'NONE',  ( 44.81606138205700063, 38.19123852234599070, 73.05501292736988717 ) ) ;
#13265 = CARTESIAN_POINT ( 'NONE',  ( 39.29254315202756231, -12.81368208888610383, 69.94417936956672577 ) ) ;
#13266 = ORIENTED_EDGE ( 'NONE', *, *, #23088, .T. ) ;
#13267 = LINE ( 'NONE', #17131, #19976 ) ;
#13268 = DIRECTION ( 'NONE',  ( 0.000000000000000000, 2.999999999999999839E-15, 1.000000000000000000 ) ) ;
#13269 = CARTESIAN_POINT ( 'NONE',  ( 36.11133435605973574, -23.61368208888610098, 72.15350918040381600 ) ) ;
#13270 = ORIENTED_EDGE ( 'NONE', *, *, #21999, .F. ) ;
#13271 = VECTOR ( 'NONE', #3959, 1000.000000000000000 ) ;
#13272 = EDGE_CURVE ( 'NONE', #23504, #17769, #9604, .T. ) ;
#13273 = FACE_OUTER_BOUND ( 'NONE', #24423, .T. ) ;
#13274 = ADVANCED_FACE ( 'NONE', ( #1093 ), #24788, .T. ) ;
#13275 = DIRECTION ( 'NONE',  ( -0.000000000000000000, -3.469446951953613400E-15, -1.000000000000000000 ) ) ;
#13276 = CARTESIAN_POINT ( 'NONE',  ( 43.81606138205700063, -33.36905983554797217, 58.95447945960771818 ) ) ;
#13277 = EDGE_CURVE ( 'NONE', #23726, #7399, #10908, .T. ) ;
#13278 = VECTOR ( 'NONE', #10131, 1000.000000000000000 ) ;
#13279 = PLANE ( 'NONE',  #3648 ) ;
#13280 = CIRCLE ( 'NONE', #11223, 0.5000000000000004441 ) ;
#13281 = AXIS2_PLACEMENT_3D ( 'NONE', #12226, #16075, #22009 ) ;
#13282 = DIRECTION ( 'NONE',  ( 0.000000000000000000, -0.4425581086832400812, 0.8967398287344626739 ) ) ;
#13283 = CARTESIAN_POINT ( 'NONE',  ( 39.02742774030101458, -15.40384086642191441, 70.49320253461759478 ) ) ;
#13284 = CARTESIAN_POINT ( 'NONE',  ( 36.68196826583682935, 0.3863179111138967392, 71.96809898377890136 ) ) ;
#13285 = ORIENTED_EDGE ( 'NONE', *, *, #16, .T. ) ;
#13286 = DIRECTION ( 'NONE',  ( 1.000000000000000000, 0.000000000000000000, 0.000000000000000000 ) ) ;
#13287 = EDGE_CURVE ( 'NONE', #23891, #6145, #20695, .T. ) ;
#13288 = CARTESIAN_POINT ( 'NONE',  ( 33.31606138205700773, 7.535758204303438568, 66.26723409915207696 ) ) ;
#13289 = ORIENTED_EDGE ( 'NONE', *, *, #8085, .F. ) ;
#13290 = ORIENTED_EDGE ( 'NONE', *, *, #22858, .T. ) ;
#13291 = VECTOR ( 'NONE', #21580, 1000.000000000000000 ) ;
#13292 = CARTESIAN_POINT ( 'NONE',  ( 40.52078840805429394, -29.00384086642191406, 72.15350918040381600 ) ) ;
#13293 = CIRCLE ( 'NONE', #2989, 0.4999999999999998890 ) ;
#13294 = CARTESIAN_POINT ( 'NONE',  ( 37.38336156205274818, -27.71368208888610241, 72.12822762946747446 ) ) ;
#13295 = CARTESIAN_POINT ( 'NONE',  ( 36.29569395875879678, -3.313682088886101607, 69.98269868914869107 ) ) ;
#13296 = VERTEX_POINT ( 'NONE', #2422 ) ;
#13297 = LINE ( 'NONE', #7361, #13599 ) ;
#13298 = CARTESIAN_POINT ( 'NONE',  ( 39.41296390513587511, -5.203840866421910683, 71.08074471024443142 ) ) ;
#13299 = CARTESIAN_POINT ( 'NONE',  ( 32.56606138205700773, 0.6124887759231013584, 82.37823623207334833 ) ) ;
#13300 = ORIENTED_EDGE ( 'NONE', *, *, #10611, .F. ) ;
#13301 = VECTOR ( 'NONE', #11829, 1000.000000000000000 ) ;
#13302 = CARTESIAN_POINT ( 'NONE',  ( 31.81606138205700418, -34.55876147765401640, 70.30501292737011454 ) ) ;
#13303 = DIRECTION ( 'NONE',  ( 0.000000000000000000, 0.3299742535180974490, -0.9439899321577398528 ) ) ;
#13304 = CARTESIAN_POINT ( 'NONE',  ( 36.29569395875881099, -8.303840866421920097, 72.77780686321129622 ) ) ;
#13305 = CARTESIAN_POINT ( 'NONE',  ( 37.42719827050449055, -22.02785702039573934, 75.80686219251248303 ) ) ;
#13306 = SURFACE_SIDE_STYLE ('',( #25115 ) ) ;
#13307 = CARTESIAN_POINT ( 'NONE',  ( 39.75915168707250302, -14.71368208888610063, 70.26145752964251301 ) ) ;
#13308 = CARTESIAN_POINT ( 'NONE',  ( 32.56606138205700773, 42.11769259596595560, 81.89079936499675227 ) ) ;
#13309 = CIRCLE ( 'NONE', #22340, 1.000000000000000888 ) ;
#13310 = CARTESIAN_POINT ( 'NONE',  ( 44.31606138205700063, 9.733755362416909307, 68.18201966341686671 ) ) ;
#13311 = VERTEX_POINT ( 'NONE', #968 ) ;
#13312 = DIRECTION ( 'NONE',  ( -1.327674326049719602E-15, 0.4425581086832399147, -0.8967398287344627850 ) ) ;
#13313 = CIRCLE ( 'NONE', #22370, 1.000000000000000888 ) ;
#13314 = CARTESIAN_POINT ( 'NONE',  ( 39.75915168707251723, -6.903840866421914413, 72.49904802271740323 ) ) ;
#13315 = SHAPE_DEFINITION_REPRESENTATION ( #15886, #14587 ) ;
#13316 = CARTESIAN_POINT ( 'NONE',  ( 33.32111138205700485, 3.997296121548431724, 6.311886478796241207 ) ) ;
#13317 = CARTESIAN_POINT ( 'NONE',  ( 39.75915168707250302, -16.71368208888609885, 70.26145752964251301 ) ) ;
#13318 = B_SPLINE_CURVE_WITH_KNOTS ( 'NONE', 3,
 ( #22743, #20822, #12600, #2651 ),
 .UNSPECIFIED., .F., .F.,
 ( 4, 4 ),
 ( 0.000000000000000000, 1.000000000000000000 ),
 .UNSPECIFIED. ) ;
#13319 = CARTESIAN_POINT ( 'NONE',  ( 32.31606138205700063, -21.26162886970023536, 44.16441745890789150 ) ) ;
#13320 = AXIS2_PLACEMENT_3D ( 'NONE', #14594, #8429, #18588 ) ;
#13321 = CARTESIAN_POINT ( 'NONE',  ( 37.80618814713138676, -19.70384086642190624, 69.62690120949091011 ) ) ;
#13322 = CARTESIAN_POINT ( 'NONE',  ( 36.72255525790973252, -5.988945345917574770, 83.28127815260972966 ) ) ;
#13323 = PRESENTATION_LAYER_ASSIGNMENT (  '', '', ( #534 ) ) ;
#13324 = CARTESIAN_POINT ( 'NONE',  ( 37.69796330110504101, -21.11368208888610454, 69.66206559358661821 ) ) ;
#13325 = VERTEX_POINT ( 'NONE', #24662 ) ;
#13326 = CARTESIAN_POINT ( 'NONE',  ( 39.12911128074873801, -28.11368208888610809, 73.69843995877326392 ) ) ;
#13327 = ORIENTED_EDGE ( 'NONE', *, *, #9587, .F. ) ;
#13328 = CARTESIAN_POINT ( 'NONE',  ( 40.31606138205700773, -11.98739464995938597, 18.25051608701495809 ) ) ;
#13329 = AXIS2_PLACEMENT_3D ( 'NONE', #8786, #10582, #768 ) ;
#13330 = CARTESIAN_POINT ( 'NONE',  ( 36.81465384343994884, 42.57231754924293909, 79.37823623207320622 ) ) ;
#13331 = CARTESIAN_POINT ( 'NONE',  ( 38.73920764526923932, -25.50384086642191406, 70.26206559358661252 ) ) ;
#13332 = ORIENTED_EDGE ( 'NONE', *, *, #21436, .T. ) ;
#13333 = VERTEX_POINT ( 'NONE', #14882 ) ;
#13334 = DIRECTION ( 'NONE',  ( -1.327674326049719602E-15, 0.4425581086832399147, -0.8967398287344627850 ) ) ;
#13335 = AXIS2_PLACEMENT_3D ( 'NONE', #16475, #18428, #757 ) ;
#13336 = DIRECTION ( 'NONE',  ( -0.1733269559585509378, 0.000000000000000000, -0.9848643390529188135 ) ) ;
#13337 = FACE_BOUND ( 'NONE', #17718, .T. ) ;
#13338 = CARTESIAN_POINT ( 'NONE',  ( 39.73277004305197124, -27.40384086642191619, 69.52238214136765748 ) ) ;
#13339 = ADVANCED_FACE ( 'NONE', ( #4976 ), #18161, .T. ) ;
#13340 = DIRECTION ( 'NONE',  ( 0.000000000000000000, -0.8212051873014208914, -0.5706330172266919076 ) ) ;
#13341 = EDGE_CURVE ( 'NONE', #2117, #21490, #18292, .T. ) ;
#13342 = DIRECTION ( 'NONE',  ( 0.000000000000000000, 2.999999999999999839E-15, 1.000000000000000000 ) ) ;
#13343 = ORIENTED_EDGE ( 'NONE', *, *, #5101, .T. ) ;
#13344 = EDGE_CURVE ( 'NONE', #17183, #24921, #3032, .T. ) ;
#13345 = ORIENTED_EDGE ( 'NONE', *, *, #24011, .T. ) ;
#13346 = CARTESIAN_POINT ( 'NONE',  ( 43.06606138205700063, 41.44123852234595518, 61.30501292736988006 ) ) ;
#13347 = PLANE ( 'NONE',  #6049 ) ;
#13348 = DIRECTION ( 'NONE',  ( -3.373073425510455500E-16, -2.999999999999999839E-15, -1.000000000000000000 ) ) ;
#13349 = VECTOR ( 'NONE', #1703, 1000.000000000000000 ) ;
#13350 = VECTOR ( 'NONE', #17863, 1000.000000000000000 ) ;
#13351 =( NAMED_UNIT ( * ) SI_UNIT ( $, .STERADIAN. ) SOLID_ANGLE_UNIT ( ) );
#13352 = DIRECTION ( 'NONE',  ( -1.000000000000000000, 0.000000000000000000, 0.000000000000000000 ) ) ;
#13353 = ORIENTED_EDGE ( 'NONE', *, *, #23403, .F. ) ;
#13354 = FACE_OUTER_BOUND ( 'NONE', #7426, .T. ) ;
#13355 = AXIS2_PLACEMENT_3D ( 'NONE', #20390, #16009, #24230 ) ;
#13356 = ADVANCED_FACE ( 'NONE', ( #8683 ), #5888, .F. ) ;
#13357 = DIRECTION ( 'NONE',  ( -1.000000000000000000, -2.952017753711455077E-15, -9.722472704681867976E-17 ) ) ;
#13358 = EDGE_LOOP ( 'NONE', ( #14739, #2941, #810, #1364 ) ) ;
#13359 = DIRECTION ( 'NONE',  ( 3.469446951953614189E-15, -1.000000000000000000, 0.000000000000000000 ) ) ;
#13360 = ORIENTED_EDGE ( 'NONE', *, *, #1531, .T. ) ;
#13361 = VERTEX_POINT ( 'NONE', #22447 ) ;
#13362 = PLANE ( 'NONE',  #4434 ) ;
#13363 = CARTESIAN_POINT ( 'NONE',  ( 37.31647492878122563, -9.313682088886098498, 70.72433947564853440 ) ) ;
#13364 = DIRECTION ( 'NONE',  ( 1.000000000000000000, 0.000000000000000000, 0.000000000000000000 ) ) ;
#13365 = CARTESIAN_POINT ( 'NONE',  ( 37.21915885897815457, -9.413682088886103472, 71.08074471024443142 ) ) ;
#13366 = ORIENTED_EDGE ( 'NONE', *, *, #3106, .T. ) ;
#13367 = EDGE_LOOP ( 'NONE', ( #21050, #13472, #9126, #3419 ) ) ;
#13368 = DIRECTION ( 'NONE',  ( -1.000000000000000000, -2.999999999999999839E-15, 0.000000000000000000 ) ) ;
#13369 = ORIENTED_EDGE ( 'NONE', *, *, #24646, .T. ) ;
#13370 = DIRECTION ( 'NONE',  ( -1.000000000000000000, 5.510910596163088391E-31, 1.836970198721029688E-16 ) ) ;
#13371 = CARTESIAN_POINT ( 'NONE',  ( 37.33957961208645315, -25.80384086642190766, 69.94417936956671156 ) ) ;
#13372 = EDGE_CURVE ( 'NONE', #21491, #1363, #987, .T. ) ;
#13373 = ADVANCED_FACE ( 'NONE', ( #24232 ), #16516, .F. ) ;
#13374 = CARTESIAN_POINT ( 'NONE',  ( 42.71157262388818054, 2.752950597436833124, 6.094617809961420996 ) ) ;
#13375 = CARTESIAN_POINT ( 'NONE',  ( 37.31647492878122563, -19.31368208888610027, 70.72433947564853440 ) ) ;
#13376 = AXIS2_PLACEMENT_3D ( 'NONE', #22766, #1254, #14652 ) ;
#13377 = ORIENTED_EDGE ( 'NONE', *, *, #23432, .T. ) ;
#13378 = EDGE_CURVE ( 'NONE', #24541, #22414, #794, .T. ) ;
#13379 = EDGE_CURVE ( 'NONE', #9429, #20085, #3951, .T. ) ;
#13380 = ORIENTED_EDGE ( 'NONE', *, *, #9920, .T. ) ;
#13381 = CARTESIAN_POINT ( 'NONE',  ( 43.06277335143801821, 3.412913593199472295, 6.350629247954049816 ) ) ;
#13382 = CARTESIAN_POINT ( 'NONE',  ( 32.56606138205700773, 43.35512946304240245, 83.12823623207320622 ) ) ;
#13383 = DIRECTION ( 'NONE',  ( -1.000000000000000000, 1.040834085586084551E-30, 3.469446951953615175E-16 ) ) ;
#13384 = CARTESIAN_POINT ( 'NONE',  ( 39.20459794252392527, -5.407735589517674413, 83.30821102113711163 ) ) ;
#13385 = CYLINDRICAL_SURFACE ( 'NONE', #21736, 0.5000000000000008882 ) ;
#13386 = CARTESIAN_POINT ( 'NONE',  ( 31.81606138205700418, 34.87886987267149408, 80.75501292736991843 ) ) ;
#13387 = EDGE_LOOP ( 'NONE', ( #9183, #12915, #16461, #8579, #7809 ) ) ;
#13388 = CARTESIAN_POINT ( 'NONE',  ( 44.81606138205700063, 38.19123852234598360, 71.05501292736988717 ) ) ;
#13389 = LINE ( 'NONE', #7454, #3313 ) ;
#13390 = ORIENTED_EDGE ( 'NONE', *, *, #11310, .T. ) ;
#13391 = VERTEX_POINT ( 'NONE', #201 ) ;
#13392 = CARTESIAN_POINT ( 'NONE',  ( 40.77203464402485622, -9.103840866421915479, 71.43714994484034264 ) ) ;
#13393 = ADVANCED_FACE ( 'NONE', ( #10487 ), #25445, .F. ) ;
#13394 = DIRECTION ( 'NONE',  ( 1.000000000000000000, 1.156482317317870344E-15, 0.000000000000000000 ) ) ;
#13395 = CARTESIAN_POINT ( 'NONE',  ( 38.37017380507020192, -16.01368208888610667, 73.11602215082116629 ) ) ;
#13396 = ORIENTED_EDGE ( 'NONE', *, *, #22081, .T. ) ;
#13397 = CARTESIAN_POINT ( 'NONE',  ( 31.81606138205700418, 40.39281886181299797, 80.75501292736983316 ) ) ;
#13398 = DIRECTION ( 'NONE',  ( 0.000000000000000000, 0.4425581086832385824, -0.8967398287344634511 ) ) ;
#13399 = CARTESIAN_POINT ( 'NONE',  ( 39.02088643472237095, -20.91368208888609814, 69.02690120949091579 ) ) ;
#13400 = ORIENTED_EDGE ( 'NONE', *, *, #23422, .F. ) ;
#13401 = CARTESIAN_POINT ( 'NONE',  ( 29.81606138205706102, -33.21365173458017495, 70.96885009038120984 ) ) ;
#13402 = PLANE ( 'NONE',  #22738 ) ;
#13403 = DIRECTION ( 'NONE',  ( -1.000000000000000000, -1.187136597504755470E-16, -8.249087426255173666E-17 ) ) ;
#13404 = DIRECTION ( 'NONE',  ( -1.000000000000000000, -2.999999999999999839E-15, 0.000000000000000000 ) ) ;
#13405 = CARTESIAN_POINT ( 'NONE',  ( 39.31564783533279694, -13.30384086642190944, 70.72433947564853440 ) ) ;
#13406 = CARTESIAN_POINT ( 'NONE',  ( 37.33957961208646736, -1.813682088886107380, 72.81632618279323310 ) ) ;
#13407 = ORIENTED_EDGE ( 'NONE', *, *, #7052, .T. ) ;
#13408 = CARTESIAN_POINT ( 'NONE',  ( 38.58254500368953188, -22.22120764818083671, 75.30501292737000085 ) ) ;
#13409 = CARTESIAN_POINT ( 'NONE',  ( 39.81606138205699352, 5.691238522346988127, 65.30501292736998664 ) ) ;
#13410 = VERTEX_POINT ( 'NONE', #14591 ) ;
#13411 = ORIENTED_EDGE ( 'NONE', *, *, #24744, .F. ) ;
#13412 = EDGE_CURVE ( 'NONE', #10709, #19565, #665, .T. ) ;
#13413 = CARTESIAN_POINT ( 'NONE',  ( 40.77203464402485622, -29.10384086642191193, 71.43714994484031422 ) ) ;
#13414 = CARTESIAN_POINT ( 'NONE',  ( 36.87297107704152666, -1.713682088886108179, 72.49904802271743165 ) ) ;
#13415 = B_SPLINE_SURFACE_WITH_KNOTS ( 'NONE', 1, 3, ( 
 ( #140, #9949, #1680, #1938 ),
 ( #3620, #11504, #23457, #7634 ),
 ( #11375, #13681, #25377, #5823 ) ),
 .UNSPECIFIED., .F., .F., .F.,
 ( 2, 1, 2 ),
 ( 4, 4 ),
 ( -0.01000000000000000021, 0.000000000000000000, 1.000000000000000000 ),
 ( 0.000000000000000000, 1.000000000000000000 ),
 .UNSPECIFIED. ) ;
#13416 = CARTESIAN_POINT ( 'NONE',  ( 39.12911128074873801, -2.113682088886108534, 73.69843995877330656 ) ) ;
#13417 = EDGE_LOOP ( 'NONE', ( #14250, #19788, #22232, #11818 ) ) ;
#13418 = CARTESIAN_POINT ( 'NONE',  ( 43.31606138205700063, -16.77230293220685198, 77.52306850662458260 ) ) ;
#13419 = CARTESIAN_POINT ( 'NONE',  ( 37.12184278917507640, -4.103840866421911038, 71.32335560751961623 ) ) ;
#13420 = DIRECTION ( 'NONE',  ( 3.717264591378870232E-16, 3.130104260698260371E-15, 1.000000000000000000 ) ) ;
#13421 = EDGE_LOOP ( 'NONE', ( #11692, #15282, #4455, #16423 ) ) ;
#13422 = LINE ( 'NONE', #17671, #20772 ) ;
#13423 = CARTESIAN_POINT ( 'NONE',  ( 43.31606138205700063, -11.65742039644128702, 17.30652615485722023 ) ) ;
#13424 = CARTESIAN_POINT ( 'NONE',  ( 40.33642880535521869, -9.303840866421909439, 69.98269868914867686 ) ) ;
#13425 = LINE ( 'NONE', #15598, #24240 ) ;
#13426 = SURFACE_STYLE_USAGE ( .BOTH. , #15600 ) ;
#13427 = CARTESIAN_POINT ( 'NONE',  ( 36.64852494920107517, -13.41368208888610525, 70.89533451361947414 ) ) ;
#13428 = DIRECTION ( 'NONE',  ( -1.000000000000000000, 0.000000000000000000, 0.000000000000000000 ) ) ;
#13429 = EDGE_CURVE ( 'NONE', #18894, #11508, #19664, .T. ) ;
#13430 = CARTESIAN_POINT ( 'NONE',  ( 47.81606138205695800, 0.8576245772853805516, -1.570935883000508460 ) ) ;
#13431 = ORIENTED_EDGE ( 'NONE', *, *, #15725, .T. ) ;
#13432 = DIRECTION ( 'NONE',  ( 1.000000000000000000, 0.000000000000000000, 0.000000000000000000 ) ) ;
#13433 = CARTESIAN_POINT ( 'NONE',  ( 37.69796330110505522, -10.50384086642191228, 73.09843995877331224 ) ) ;
#13434 = APPLICATION_PROTOCOL_DEFINITION ( 'draft international standard', 'automotive_design', 1998, #24577 ) ;
#13435 = PLANE ( 'NONE',  #19888 ) ;
#13436 = CARTESIAN_POINT ( 'NONE',  ( 38.26194895904383486, -19.01368208888610312, 69.64448340153877837 ) ) ;
#13437 = DIRECTION ( 'NONE',  ( 0.000000000000000000, 0.6568589528324747517, -0.7540134720837718962 ) ) ;
#13438 = CARTESIAN_POINT ( 'NONE',  ( 38.37017380507018771, -15.60384086642190837, 69.64448340153877837 ) ) ;
#13439 = CARTESIAN_POINT ( 'NONE',  ( 42.96606138205694236, 6.105630034208211931, 5.871938670042847974 ) ) ;
#13440 = EDGE_CURVE ( 'NONE', #19403, #20407, #23659, .T. ) ;
#13441 = CARTESIAN_POINT ( 'NONE',  ( 36.64852494920107517, -15.41368208888610525, 70.89533451361947414 ) ) ;
#13442 = ORIENTED_EDGE ( 'NONE', *, *, #2654, .T. ) ;
#13443 = CARTESIAN_POINT ( 'NONE',  ( 36.89935272106204422, -25.21368208888610241, 69.52238214136765748 ) ) ;
#13444 = ORIENTED_EDGE ( 'NONE', *, *, #6367, .F. ) ;
#13445 = CARTESIAN_POINT ( 'NONE',  ( 32.81606138205700773, -1.963190818658398173, 19.89143565483009013 ) ) ;
#13446 = DIRECTION ( 'NONE',  ( -1.836970198721029688E-16, -2.999999999999999839E-15, -1.000000000000000000 ) ) ;
#13447 = CARTESIAN_POINT ( 'NONE',  ( 37.31647492878124694, -26.30384086642190766, 72.03616607671141026 ) ) ;
#13448 = EDGE_LOOP ( 'NONE', ( #19558, #2676, #8539, #23816 ) ) ;
#13449 = ORIENTED_EDGE ( 'NONE', *, *, #2457, .F. ) ;
#13450 = DIRECTION ( 'NONE',  ( 1.000000000000000000, 6.071532165918830747E-16, -1.734723475976829774E-16 ) ) ;
#13451 = FACE_OUTER_BOUND ( 'NONE', #17973, .T. ) ;
#13452 = LINE ( 'NONE', #11285, #21746 ) ;
#13453 = CARTESIAN_POINT ( 'NONE',  ( 39.98359781491296161, 0.7961591335780872081, 70.89533451361948835 ) ) ;
#13454 = CARTESIAN_POINT ( 'NONE',  ( 41.06606138205702194, -19.40517585842701820, 23.66972737280834238 ) ) ;
#13455 = ADVANCED_FACE ( 'NONE', ( #7824 ), #15670, .T. ) ;
#13456 = DIRECTION ( 'NONE',  ( 0.000000000000000000, 0.6595716529892420299, -0.7516416929448758166 ) ) ;
#13457 = VECTOR ( 'NONE', #9490, 1000.000000000000000 ) ;
#13458 = EDGE_LOOP ( 'NONE', ( #21442, #16446, #9590, #11439 ) ) ;
#13459 = ORIENTED_EDGE ( 'NONE', *, *, #21287, .T. ) ;
#13460 = AXIS2_PLACEMENT_3D ( 'NONE', #11632, #9823, #17678 ) ;
#13461 = AXIS2_PLACEMENT_3D ( 'NONE', #23721, #2080, #17950 ) ;
#13462 = DIRECTION ( 'NONE',  ( -1.000000000000000000, -2.168404344971055214E-16, 1.734723475976814737E-16 ) ) ;
#13463 = DIRECTION ( 'NONE',  ( -1.836970198721029688E-16, -2.999999999999999839E-15, -1.000000000000000000 ) ) ;
#13464 = CARTESIAN_POINT ( 'NONE',  ( 40.05245289102395390, -29.10876147765230115, 71.40796565871902146 ) ) ;
#13465 =( NAMED_UNIT ( * ) SI_UNIT ( $, .STERADIAN. ) SOLID_ANGLE_UNIT ( ) );
#13466 = CARTESIAN_POINT ( 'NONE',  ( 32.81606138205700773, -34.55876147765401640, 70.30501292737011454 ) ) ;
#13467 = VERTEX_POINT ( 'NONE', #23776 ) ;
#13468 = LINE ( 'NONE', #3540, #19686 ) ;
#13469 = CARTESIAN_POINT ( 'NONE',  ( 33.66606138205695231, 3.409598742320806952, 3.426245460917042074 ) ) ;
#13470 = CARTESIAN_POINT ( 'NONE',  ( 45.81606138205706458, -34.54722833698617990, 70.28164373264664277 ) ) ;
#13471 = CARTESIAN_POINT ( 'NONE',  ( 38.63098279924290068, -8.703840866421911571, 72.53360434286905445 ) ) ;
#13472 = ORIENTED_EDGE ( 'NONE', *, *, #3578, .T. ) ;
#13473 = CARTESIAN_POINT ( 'NONE',  ( 38.41621794735363693, -36.60729675983900222, 83.30501292737011454 ) ) ;
#13474 = ORIENTED_EDGE ( 'NONE', *, *, #6000, .F. ) ;
#13475 = ORIENTED_EDGE ( 'NONE', *, *, #7695, .F. ) ;
#13476 = VECTOR ( 'NONE', #16903, 1000.000000000000227 ) ;
#13477 = LINE ( 'NONE', #9999, #15529 ) ;
#13478 = CARTESIAN_POINT ( 'NONE',  ( 39.41296390513587511, -14.41368208888610347, 71.67976084211551324 ) ) ;
#13479 = VECTOR ( 'NONE', #11, 1000.000000000000000 ) ;
#13480 = AXIS2_PLACEMENT_3D ( 'NONE', #5614, #3674, #11558 ) ;
#13481 = CARTESIAN_POINT ( 'NONE',  ( 37.60469502381300089, -11.21368208888610241, 70.49320253461759478 ) ) ;
#13482 = ORIENTED_EDGE ( 'NONE', *, *, #25221, .T. ) ;
#13483 = VERTEX_POINT ( 'NONE', #23519 ) ;
#13484 = CARTESIAN_POINT ( 'NONE',  ( 31.56606138205707168, -38.42645682328038248, 63.90656833300437256 ) ) ;
#13485 = CARTESIAN_POINT ( 'NONE',  ( 41.81606138205700063, -21.26162886970023536, 44.16441745890789150 ) ) ;
#13486 = VERTEX_POINT ( 'NONE', #14468 ) ;
#13487 = DIRECTION ( 'NONE',  ( -1.000000000000000000, 0.000000000000000000, 0.000000000000000000 ) ) ;
#13488 = CARTESIAN_POINT ( 'NONE',  ( 39.75915168707251723, -18.90384086642190553, 72.49904802271738902 ) ) ;
#13489 = CARTESIAN_POINT ( 'NONE',  ( 42.99635608599476200, 2.840112565366839092, 6.103054897711724713 ) ) ;
#13490 = EDGE_CURVE ( 'NONE', #4607, #3296, #10013, .T. ) ;
#13491 = CARTESIAN_POINT ( 'NONE',  ( 37.38336156205274818, -19.71368208888610596, 72.12822762946750288 ) ) ;
#13492 = VERTEX_POINT ( 'NONE', #17875 ) ;
#13493 = LINE ( 'NONE', #21344, #19051 ) ;
#13494 = CARTESIAN_POINT ( 'NONE',  ( 40.31606138205700063, 5.691238522346998785, 68.80501292736998664 ) ) ;
#13495 = VECTOR ( 'NONE', #20189, 1000.000000000000000 ) ;
#13496 = CARTESIAN_POINT ( 'NONE',  ( 35.81606138205700063, 5.691238522346998785, 68.80501292736998664 ) ) ;
#13497 = AXIS2_PLACEMENT_3D ( 'NONE', #10488, #16136, #22065 ) ;
#13498 = VECTOR ( 'NONE', #10143, 1000.000000000000114 ) ;
#13499 = CARTESIAN_POINT ( 'NONE',  ( 38.96303889229209716, -5.302308566866229533, 82.80464595504712122 ) ) ;
#13500 = CARTESIAN_POINT ( 'NONE',  ( 32.81606138205700773, 35.92314894770293421, 79.37823623207323465 ) ) ;
#13501 = B_SPLINE_CURVE_WITH_KNOTS ( 'NONE', 3,
 ( #326, #14006, #14258, #12337 ),
 .UNSPECIFIED., .F., .F.,
 ( 4, 4 ),
 ( 0.000000000000000000, 1.000000000000000000 ),
 .UNSPECIFIED. ) ;
#13502 = DIRECTION ( 'NONE',  ( -1.000000000000000000, -2.440719103442460911E-15, -1.328886038262200866E-15 ) ) ;
#13503 = EDGE_CURVE ( 'NONE', #15622, #7399, #17741, .T. ) ;
#13504 = EDGE_LOOP ( 'NONE', ( #3551, #22557, #4660, #16905 ) ) ;
#13505 = EDGE_CURVE ( 'NONE', #22756, #7686, #7957, .T. ) ;
#13506 = DIRECTION ( 'NONE',  ( 0.000000000000000000, -0.7540134720837687876, -0.6568589528324780824 ) ) ;
#13507 = VERTEX_POINT ( 'NONE', #6141 ) ;
#13508 = EDGE_LOOP ( 'NONE', ( #13475, #15944, #3994 ) ) ;
#13509 = CARTESIAN_POINT ( 'NONE',  ( 40.55423172469004101, -9.203840866421915123, 70.70992431699450265 ) ) ;
#13510 = ADVANCED_FACE ( 'NONE', ( #15802 ), #11955, .T. ) ;
#13511 = EDGE_CURVE ( 'NONE', #22911, #21429, #7994, .T. ) ;
#13512 = CARTESIAN_POINT ( 'NONE',  ( 44.81606138205700063, -24.55876147765401285, 70.30501292737008612 ) ) ;
#13513 = CARTESIAN_POINT ( 'NONE',  ( 39.38009889167650357, -14.21368208888610773, 72.75271321436731853 ) ) ;
#13514 = AXIS2_PLACEMENT_3D ( 'NONE', #4478, #462, #10024 ) ;
#13515 =( NAMED_UNIT ( * ) SI_UNIT ( $, .STERADIAN. ) SOLID_ANGLE_UNIT ( ) );
#13516 = ORIENTED_EDGE ( 'NONE', *, *, #15663, .F. ) ;
#13517 = PLANE ( 'NONE',  #4352 ) ;
#13518 = CARTESIAN_POINT ( 'NONE',  ( 43.31606138205700063, 2.761903742731119049, 12.21527246050395377 ) ) ;
#13519 = EDGE_CURVE ( 'NONE', #5254, #17216, #10373, .T. ) ;
#13520 = CARTESIAN_POINT ( 'NONE',  ( 38.37017380507020192, -24.01368208888611022, 73.71602215082113219 ) ) ;
#13521 = EDGE_CURVE ( 'NONE', #21012, #25135, #684, .T. ) ;
#13522 =( NAMED_UNIT ( * ) SI_UNIT ( $, .STERADIAN. ) SOLID_ANGLE_UNIT ( ) );
#13523 = DIRECTION ( 'NONE',  ( 0.000000000000000000, -0.5706330172266952383, 0.8212051873014186709 ) ) ;
#13524 = DIRECTION ( 'NONE',  ( 1.000000000000000000, 1.518641380243644581E-16, 1.055262346480601087E-16 ) ) ;
#13525 = CIRCLE ( 'NONE', #7344, 0.2000000000000057288 ) ;
#13526 = DIRECTION ( 'NONE',  ( 0.000000000000000000, -0.3299742535180974490, 0.9439899321577398528 ) ) ;
#13527 = DIRECTION ( 'NONE',  ( 1.218693434051482139E-16, -0.4425581086832393041, 0.8967398287344630070 ) ) ;
#13528 = CARTESIAN_POINT ( 'NONE',  ( 37.69225076346193504, -9.803840866421911215, 70.42958956619168021 ) ) ;
#13529 = CARTESIAN_POINT ( 'NONE',  ( 39.02742774030102879, -28.21368208888610596, 72.26730301774232146 ) ) ;
#13530 = AXIS2_PLACEMENT_3D ( 'NONE', #15485, #3253, #15234 ) ;
#13531 = ORIENTED_EDGE ( 'NONE', *, *, #20976, .F. ) ;
#13532 = DIRECTION ( 'NONE',  ( 0.000000000000000000, 2.775557561562888984E-15, 1.000000000000000000 ) ) ;
#13533 = LINE ( 'NONE', #7616, #23839 ) ;
#13534 = ORIENTED_EDGE ( 'NONE', *, *, #8621, .F. ) ;
#13535 = VERTEX_POINT ( 'NONE', #19913 ) ;
#13536 = CARTESIAN_POINT ( 'NONE',  ( 40.52078840805429394, -27.00384086642191761, 72.15350918040381600 ) ) ;
#13537 = VECTOR ( 'NONE', #3594, 1000.000000000000000 ) ;
#13538 = CARTESIAN_POINT ( 'NONE',  ( 39.51027997493896748, -28.51368208888610667, 71.32335560751960202 ) ) ;
#13539 = CARTESIAN_POINT ( 'NONE',  ( 40.26954217208371034, -0.7136820888861000745, 69.89063713639259845 ) ) ;
#13540 = ORIENTED_EDGE ( 'NONE', *, *, #13503, .F. ) ;
#13541 = PLANE ( 'NONE',  #14007 ) ;
#13542 = CARTESIAN_POINT ( 'NONE',  ( 38.26194895904384197, -6.603840866421913702, 72.51602215082118619 ) ) ;
#13543 = CIRCLE ( 'NONE', #18897, 1.750000000000001554 ) ;
#13544 = FILL_AREA_STYLE_COLOUR ( '', #11852 ) ;
#13545 = ORIENTED_EDGE ( 'NONE', *, *, #10524, .T. ) ;
#13546 = CARTESIAN_POINT ( 'NONE',  ( 30.81606138205700418, -0.6071811381869983704, 80.05501292737000085 ) ) ;
#13547 = DIRECTION ( 'NONE',  ( 1.734723475976814737E-16, -1.000000000000000000, 3.491481338843135327E-15 ) ) ;
#13548 = CARTESIAN_POINT ( 'NONE',  ( 40.77203464402485622, -13.10384086642191548, 71.43714994484032843 ) ) ;
#13549 = DIRECTION ( 'NONE',  ( 2.595751990468335074E-30, 1.000000000000000000, -3.491481338843135327E-15 ) ) ;
#13550 = CIRCLE ( 'NONE', #23411, 0.5000000000000004441 ) ;
#13551 = CARTESIAN_POINT ( 'NONE',  ( 36.31606138205700773, -21.45740613484710479, 28.95788407061096237 ) ) ;
#13552 = CARTESIAN_POINT ( 'NONE',  ( 38.93415946300897446, -16.11368208888611164, 73.09843995877329803 ) ) ;
#13553 = FACE_BOUND ( 'NONE', #20866, .T. ) ;
#13554 = DIRECTION ( 'NONE',  ( 0.000000000000000000, -0.7540134720837717852, -0.6568589528324746407 ) ) ;
#13555 = ORIENTED_EDGE ( 'NONE', *, *, #9912, .F. ) ;
#13556 = CARTESIAN_POINT ( 'NONE',  ( 43.31606138205700063, 4.529600202371326212, 14.05245759722139454 ) ) ;
#13557 = ADVANCED_FACE ( 'NONE', ( #14362 ), #22086, .F. ) ;
#13558 = CARTESIAN_POINT ( 'NONE',  ( 38.26194895904384907, -0.6038408664219147015, 73.11602215082118050 ) ) ;
#13559 = ADVANCED_FACE ( 'NONE', ( #4194 ), #18359, .T. ) ;
#13560 = ITEM_DEFINED_TRANSFORMATION ( 'NONE', 'NONE', #19529,  #2000 ) ;
#13561 = CARTESIAN_POINT ( 'NONE',  ( 33.56477571746444255, 3.418883076854433600, 6.349191931652259591 ) ) ;
#13562 = VECTOR ( 'NONE', #8981, 1000.000000000000000 ) ;
#13563 = CARTESIAN_POINT ( 'NONE',  ( 37.25202387243752611, -17.21368208888610241, 70.00779233799262613 ) ) ;
#13564 = AXIS2_PLACEMENT_3D ( 'NONE', #19825, #24301, #20206 ) ;
#13565 = DIRECTION ( 'NONE',  ( -1.000000000000000000, 0.000000000000000000, 0.000000000000000000 ) ) ;
#13566 = CARTESIAN_POINT ( 'NONE',  ( 36.87297107704149823, -19.90384086642190198, 70.26145752964252722 ) ) ;
#13567 = CARTESIAN_POINT ( 'NONE',  ( 36.31606138205700063, -7.108955154158179468, 82.62193108360246185 ) ) ;
#13568 = VECTOR ( 'NONE', #4443, 1000.000000000000000 ) ;
#13569 = CARTESIAN_POINT ( 'NONE',  ( 38.93415946300897446, -18.11368208888611164, 73.09843995877329803 ) ) ;
#13570 = ORIENTED_EDGE ( 'NONE', *, *, #11243, .T. ) ;
#13571 = CARTESIAN_POINT ( 'NONE',  ( 37.61123632939165873, -19.91368208888610880, 73.73360434286898624 ) ) ;
#13572 = ORIENTED_EDGE ( 'NONE', *, *, #2699, .F. ) ;
#13573 = DIRECTION ( 'NONE',  ( 1.000000000000000000, 8.673617379884027583E-16, 0.000000000000000000 ) ) ;
#13574 = DIRECTION ( 'NONE',  ( 2.690219486203388234E-15, -0.8967398287344627850, -0.4425581086832399147 ) ) ;
#13575 = CARTESIAN_POINT ( 'NONE',  ( 37.25260217561390874, -26.00384086642191406, 70.97781676520601479 ) ) ;
#13576 = CIRCLE ( 'NONE', #14402, 1.750000000000001554 ) ;
#13577 = VERTEX_POINT ( 'NONE', #14488 ) ;
#13578 = EDGE_LOOP ( 'NONE', ( #12431, #5778, #16063, #24735 ) ) ;
#13579 = CARTESIAN_POINT ( 'NONE',  ( 39.63762123564960405, -28.98311505855621206, 70.81515399290854873 ) ) ;
#13580 = CARTESIAN_POINT ( 'NONE',  ( 45.61606138205700489, 2.823374736507280597E-13, 81.37823623207336254 ) ) ;
#13581 = DIRECTION ( 'NONE',  ( -2.048868001712899108E-15, 0.6595716529892353686, -0.7516416929448815898 ) ) ;
#13582 = CARTESIAN_POINT ( 'NONE',  ( 39.64521430340305841, -28.80384086642192187, 73.30173637941817333 ) ) ;
#13583 = VECTOR ( 'NONE', #3866, 1000.000000000000000 ) ;
#13584 = CARTESIAN_POINT ( 'NONE',  ( 43.31606138205700063, -16.77230293220685198, 77.52306850662458260 ) ) ;
#13585 = CARTESIAN_POINT ( 'NONE',  ( 37.61123632939165873, -3.913682088886108357, 73.73360434286902887 ) ) ;
#13586 = VECTOR ( 'NONE', #17934, 1000.000000000000000 ) ;
#13587 = FACE_OUTER_BOUND ( 'NONE', #24274, .T. ) ;
#13588 = ORIENTED_EDGE ( 'NONE', *, *, #11356, .T. ) ;
#13589 = ADVANCED_FACE ( 'NONE', ( #14113 ), #22346, .T. ) ;
#13590 = ORIENTED_EDGE ( 'NONE', *, *, #5799, .T. ) ;
#13591 = APPLICATION_CONTEXT ( 'automotive_design' ) ;
#13592 = EDGE_CURVE ( 'NONE', #16794, #4227, #16157, .T. ) ;
#13593 = LINE ( 'NONE', #19511, #15361 ) ;
#13594 = FACE_OUTER_BOUND ( 'NONE', #3672, .T. ) ;
#13595 = EDGE_CURVE ( 'NONE', #21859, #8869, #4242, .T. ) ;
#13596 = CARTESIAN_POINT ( 'NONE',  ( 39.38009889167648936, -23.40384086642190908, 70.00779233799262613 ) ) ;
#13597 = CARTESIAN_POINT ( 'NONE',  ( 33.31606138205700773, 7.611641054560886133, 65.67022133066943468 ) ) ;
#13598 = ORIENTED_EDGE ( 'NONE', *, *, #3317, .F. ) ;
#13599 = VECTOR ( 'NONE', #15464, 1000.000000000000000 ) ;
#13600 = DIRECTION ( 'NONE',  ( 1.000000000000000000, 0.000000000000000000, 0.000000000000000000 ) ) ;
#13601 = AXIS2_PLACEMENT_3D ( 'NONE', #14419, #23940, #10060 ) ;
#13602 = CARTESIAN_POINT ( 'NONE',  ( 30.81606138205697931, 1.361611432489137741, -2.592146606185725677 ) ) ;
#13603 = FACE_OUTER_BOUND ( 'NONE', #23608, .T. ) ;
#13604 = CARTESIAN_POINT ( 'NONE',  ( 39.24876120206129571, -8.903840866421910860, 72.12822762946750288 ) ) ;
#13605 = VERTEX_POINT ( 'NONE', #2498 ) ;
#13606 = ADVANCED_FACE ( 'NONE', ( #6386 ), #4450, .T. ) ;
#13607 = DIRECTION ( 'NONE',  ( 6.938893903907221278E-15, -1.000000000000000000, 0.000000000000000000 ) ) ;
#13608 = ORIENTED_EDGE ( 'NONE', *, *, #1022, .F. ) ;
#13609 = ORIENTED_EDGE ( 'NONE', *, *, #21858, .T. ) ;
#13610 = DIRECTION ( 'NONE',  ( -2.690219486203388234E-15, 0.8967398287344627850, 0.4425581086832399147 ) ) ;
#13611 = CARTESIAN_POINT ( 'NONE',  ( 38.73920764526925353, -12.11368208888610098, 72.49843995877330372 ) ) ;
#13612 = CARTESIAN_POINT ( 'NONE',  ( 37.38336156205274818, -13.71368208888610241, 72.12822762946750288 ) ) ;
#13613 = ORIENTED_EDGE ( 'NONE', *, *, #623, .F. ) ;
#13614 = VERTEX_POINT ( 'NONE', #12579 ) ;
#13615 = DIRECTION ( 'NONE',  ( -1.734723475976805122E-16, -3.491481338843134933E-15, -1.000000000000000000 ) ) ;
#13616 = VERTEX_POINT ( 'NONE', #187 ) ;
#13617 = DIRECTION ( 'NONE',  ( -2.690219486203388234E-15, 0.8967398287344627850, 0.4425581086832399147 ) ) ;
#13618 = CARTESIAN_POINT ( 'NONE',  ( 38.37017380507018771, -19.60384086642191193, 69.64448340153877837 ) ) ;
#13619 = VECTOR ( 'NONE', #15845, 1000.000000000000227 ) ;
#13620 = DIRECTION ( 'NONE',  ( 0.000000000000000000, 6.938893903907222067E-15, 1.000000000000000000 ) ) ;
#13621 = CARTESIAN_POINT ( 'NONE',  ( 37.12184278917507640, -17.51368208888609956, 71.43714994484034264 ) ) ;
#13622 = VECTOR ( 'NONE', #5740, 1000.000000000000000 ) ;
#13623 = VERTEX_POINT ( 'NONE', #2251 ) ;
#13624 = DIRECTION ( 'NONE',  ( 1.000000000000000000, 0.000000000000000000, -0.000000000000000000 ) ) ;
#13625 = CARTESIAN_POINT ( 'NONE',  ( 39.38009889167650357, -16.21368208888610596, 72.75271321436731853 ) ) ;
#13626 = CARTESIAN_POINT ( 'NONE',  ( 32.31606138205700063, 10.29926546647973851, 68.67466387804121553 ) ) ;
#13627 = CARTESIAN_POINT ( 'NONE',  ( 46.81606138205697931, -6.570990706613046406, -2.335727660491067503 ) ) ;
#13628 = CARTESIAN_POINT ( 'NONE',  ( 40.30346352106939634, -6.945422957003676956, 83.16042775478545934 ) ) ;
#13629 = CARTESIAN_POINT ( 'NONE',  ( 40.56606138205697931, -5.948051402551118194, 9.959574150503843981 ) ) ;
#13630 = PRODUCT_DEFINITION_SHAPE ( 'NONE', 'NONE',  #17663 ) ;
#13631 = CARTESIAN_POINT ( 'NONE',  ( 40.31606138205700773, 37.94123852234599781, 74.30501292736988717 ) ) ;
#13632 = VERTEX_POINT ( 'NONE', #20032 ) ;
#13633 = ADVANCED_FACE ( 'NONE', ( #8065 ), #17983, .F. ) ;
#13634 = CARTESIAN_POINT ( 'NONE',  ( 43.31606138205700773, -19.28757846107943763, 24.56123906878952567 ) ) ;
#13635 = ORIENTED_EDGE ( 'NONE', *, *, #6858, .F. ) ;
#13636 = ORIENTED_EDGE ( 'NONE', *, *, #21945, .F. ) ;
#13637 = VECTOR ( 'NONE', #8198, 1000.000000000000000 ) ;
#13638 = CARTESIAN_POINT ( 'NONE',  ( 40.52078840805429394, -11.00384086642191406, 72.15350918040385864 ) ) ;
#13639 = ORIENTED_EDGE ( 'NONE', *, *, #7068, .T. ) ;
#13640 = DIRECTION ( 'NONE',  ( 7.071067811865491110E-16, -0.9008287146801832179, 0.4341746501209495790 ) ) ;
#13641 = CARTESIAN_POINT ( 'NONE',  ( 36.49096545463212493, -17.51368208888610667, 71.43714994484034264 ) ) ;
#13642 = ORIENTED_EDGE ( 'NONE', *, *, #18681, .T. ) ;
#13643 = LINE ( 'NONE', #11727, #3080 ) ;
#13644 = CARTESIAN_POINT ( 'NONE',  ( 42.06606138205700063, 47.04446929126260102, 82.37823623207320622 ) ) ;
#13645 = CARTESIAN_POINT ( 'NONE',  ( 39.02088643472237095, -18.91368208888609814, 69.02690120949091579 ) ) ;
#13646 = ORIENTED_EDGE ( 'NONE', *, *, #21829, .F. ) ;
#13647 = DIRECTION ( 'NONE',  ( 1.000000000000000000, 1.000000000000000078E-15, 0.000000000000000000 ) ) ;
#13648 = CARTESIAN_POINT ( 'NONE',  ( 35.64099152588522657, 1.392818861812999964, 84.30501292737000085 ) ) ;
#13649 = LINE ( 'NONE', #101, #1743 ) ;
#13650 = EDGE_CURVE ( 'NONE', #22400, #8692, #16035, .T. ) ;
#13651 = EDGE_CURVE ( 'NONE', #21293, #3785, #17398, .T. ) ;
#13652 = AXIS2_PLACEMENT_3D ( 'NONE', #5645, #21361, #11589 ) ;
#13653 = FACE_OUTER_BOUND ( 'NONE', #17452, .T. ) ;
#13654 = ADVANCED_FACE ( 'NONE', ( #4582 ), #6252, .T. ) ;
#13655 = CARTESIAN_POINT ( 'NONE',  ( 40.31606138205702194, -20.48383445069736197, 23.59578481461660004 ) ) ;
#13656 = COLOUR_RGB ( '', 0.31764706, 0.68627451, 0.89019608) ;
#13657 = DIRECTION ( 'NONE',  ( 1.000000000000000000, 0.000000000000000000, 0.000000000000000000 ) ) ;
#13658 = CARTESIAN_POINT ( 'NONE',  ( 38.37017380507018771, -13.60384086642191193, 70.24448340153875847 ) ) ;
#13659 = CARTESIAN_POINT ( 'NONE',  ( 38.73920764526925353, -28.11368208888610454, 72.49843995877328950 ) ) ;
#13660 = ORIENTED_EDGE ( 'NONE', *, *, #18319, .T. ) ;
#13661 = CARTESIAN_POINT ( 'NONE',  ( 39.31606138205700063, 12.69123852234700678, 71.30501292736997243 ) ) ;
#13662 = CARTESIAN_POINT ( 'NONE',  ( 32.81606138205700773, 3.172506336381830661, 12.50058896911730066 ) ) ;
#13663 = ORIENTED_EDGE ( 'NONE', *, *, #623, .T. ) ;
#13664 = VERTEX_POINT ( 'NONE', #20294 ) ;
#13665 = CARTESIAN_POINT ( 'NONE',  ( 39.98359781491296161, -1.203840866421911127, 70.89533451361947414 ) ) ;
#13666 = CARTESIAN_POINT ( 'NONE',  ( 38.37017380507020192, -24.01368208888609956, 72.51602215082114355 ) ) ;
#13667 = CARTESIAN_POINT ( 'NONE',  ( 39.12911128074873801, -6.113682088886108978, 73.69843995877330656 ) ) ;
#13668 = EDGE_LOOP ( 'NONE', ( #6878, #18709, #5913, #16967 ) ) ;
#13669 = DIRECTION ( 'NONE',  ( 2.690219486203388234E-15, -0.8967398287344627850, -0.4425581086832399147 ) ) ;
#13670 = AXIS2_PLACEMENT_3D ( 'NONE', #16198, #22507, #4489 ) ;
#13671 = CARTESIAN_POINT ( 'NONE',  ( 38.37017380507018771, -7.603840866421910150, 70.24448340153877268 ) ) ;
#13672 = CARTESIAN_POINT ( 'NONE',  ( 28.81606138205695444, -23.19619402982950263, 47.16846523730000484 ) ) ;
#13673 = ORIENTED_EDGE ( 'NONE', *, *, #24317, .F. ) ;
#13674 = CARTESIAN_POINT ( 'NONE',  ( 32.81606138205700773, -40.62725863591898445, 68.52362519861142687 ) ) ;
#13675 = CARTESIAN_POINT ( 'NONE',  ( 43.81606138205700063, 4.529600202371326212, 14.05245759722139454 ) ) ;
#13676 = CIRCLE ( 'NONE', #24331, 12.59999999999999964 ) ;
#13677 = CARTESIAN_POINT ( 'NONE',  ( 36.89935272106205133, -10.40384086642191797, 73.23812341099225875 ) ) ;
#13678 = DIRECTION ( 'NONE',  ( -1.809068767804384992E-15, -1.000000000000000000, 3.491481338843135327E-15 ) ) ;
#13679 = DIRECTION ( 'NONE',  ( -1.000000000000000000, -3.091505625455828697E-15, -4.515976121274771690E-17 ) ) ;
#13680 = CARTESIAN_POINT ( 'NONE',  ( 36.68196826583682935, -15.61368208888610454, 71.96809898377888715 ) ) ;
#13681 = CARTESIAN_POINT ( 'NONE',  ( 33.88977883057645357, 3.189440312111338383, 6.370184205214554751 ) ) ;
#13682 = CIRCLE ( 'NONE', #23540, 3.000000000000002665 ) ;
#13683 = CARTESIAN_POINT ( 'NONE',  ( 38.31606138205700063, 38.69123852234599781, 71.30501292737000085 ) ) ;
#13684 = EDGE_CURVE ( 'NONE', #17867, #2806, #2628, .T. ) ;
#13685 = ADVANCED_FACE ( 'NONE', ( #4330 ), #12194, .F. ) ;
#13686 = DIRECTION ( 'NONE',  ( 0.000000000000000000, 1.000000000000000000, -2.999999999999999839E-15 ) ) ;
#13687 = CARTESIAN_POINT ( 'NONE',  ( 36.49096545463212493, -0.1038408664219107880, 71.32335560751963044 ) ) ;
#13688 = LINE ( 'NONE', #386, #16183 ) ;
#13689 = CARTESIAN_POINT ( 'NONE',  ( 38.93415946300897446, -16.11368208888611164, 73.09843995877329803 ) ) ;
#13690 = CARTESIAN_POINT ( 'NONE',  ( 40.31606138205701484, -23.16691978223481385, 31.29201591705069063 ) ) ;
#13691 = VECTOR ( 'NONE', #15664, 1000.000000000000000 ) ;
#13692 = EDGE_CURVE ( 'NONE', #7151, #16594, #2219, .T. ) ;
#13693 = CARTESIAN_POINT ( 'NONE',  ( 39.75915168707251723, -20.90384086642190553, 72.49904802271738902 ) ) ;
#13694 = CARTESIAN_POINT ( 'NONE',  ( 38.31606138205700063, -33.30876147765400219, 71.30501292737024244 ) ) ;
#13695 = VECTOR ( 'NONE', #9107, 1000.000000000000000 ) ;
#13696 = CARTESIAN_POINT ( 'NONE',  ( 37.33957961208646736, -11.81368208888610916, 72.81632618279321889 ) ) ;
#13697 = ORIENTED_EDGE ( 'NONE', *, *, #23591, .T. ) ;
#13698 = CARTESIAN_POINT ( 'NONE',  ( 40.55423172469004811, -24.41368208888610880, 72.05058123536539938 ) ) ;
#13699 = EDGE_LOOP ( 'NONE', ( #12168, #20199, #10176, #19750 ) ) ;
#13700 = DIRECTION ( 'NONE',  ( -2.515133600231165483E-15, 0.7516416929448815898, 0.6595716529892353686 ) ) ;
#13701 = CARTESIAN_POINT ( 'NONE',  ( 31.81606138205700418, -36.10876147765401356, 70.30501292737011454 ) ) ;
#13702 = CARTESIAN_POINT ( 'NONE',  ( 38.26194895904384197, -22.60384086642191548, 72.51602215082118619 ) ) ;
#13703 = ORIENTED_EDGE ( 'NONE', *, *, #23212, .F. ) ;
#13704 = ADVANCED_FACE ( 'NONE', ( #7143 ), #10884, .F. ) ;
#13705 = VERTEX_POINT ( 'NONE', #24887 ) ;
#13706 = DIRECTION ( 'NONE',  ( 0.000000000000000000, -1.000000000000000000, 6.123233995736769734E-17 ) ) ;
#13707 = DIRECTION ( 'NONE',  ( 1.000000000000000000, 2.999999999999999839E-15, 0.000000000000000000 ) ) ;
#13709 = CIRCLE ( 'NONE', #14531, 0.5000000000000004441 ) ;
#13708 = DIRECTION ( 'NONE',  ( -1.327674326049721180E-15, 0.4425581086832404143, -0.8967398287344625629 ) ) ;
#13710 = CARTESIAN_POINT ( 'NONE',  ( 38.82593461698265003, 1.296159133578084210, 73.13360434286906298 ) ) ;
#13711 = VECTOR ( 'NONE', #12471, 1000.000000000000227 ) ;
#13712 = DIRECTION ( 'NONE',  ( -1.000000000000000000, 0.000000000000000000, 0.000000000000000000 ) ) ;
#13713 = CARTESIAN_POINT ( 'NONE',  ( 35.86008812008917346, 0.4863179111138961064, 71.43714994484035685 ) ) ;
#13714 = VECTOR ( 'NONE', #4036, 1000.000000000000000 ) ;
#13715 = LINE ( 'NONE', #40, #19672 ) ;
#13716 = ORIENTED_EDGE ( 'NONE', *, *, #17120, .F. ) ;
#13717 = EDGE_LOOP ( 'NONE', ( #15328, #6185, #20495, #14525 ) ) ;
#13718 = DIRECTION ( 'NONE',  ( 1.000000000000000000, 2.973811673103095397E-15, 0.000000000000000000 ) ) ;
#13719 = LINE ( 'NONE', #7925, #20045 ) ;
#13720 = AXIS2_PLACEMENT_3D ( 'NONE', #15924, #21860, #18255 ) ;
#13721 = CARTESIAN_POINT ( 'NONE',  ( 36.80608444377002542, -18.30384086642191122, 72.40698646996133903 ) ) ;
#13722 = LINE ( 'NONE', #17588, #13291 ) ;
#13723 = ORIENTED_EDGE ( 'NONE', *, *, #16632, .T. ) ;
#13724 = DIRECTION ( 'NONE',  ( -1.000000000000000000, -0.000000000000000000, 0.000000000000000000 ) ) ;
#13725 = CIRCLE ( 'NONE', #7551, 1.250000000000000888 ) ;
#13726 = FACE_OUTER_BOUND ( 'NONE', #16691, .T. ) ;
#13727 = FACE_OUTER_BOUND ( 'NONE', #1097, .T. ) ;
#13728 = CARTESIAN_POINT ( 'NONE',  ( 38.00113996487112189, -5.703840866421911571, 70.22690120949091863 ) ) ;
#13729 = ORIENTED_EDGE ( 'NONE', *, *, #10053, .T. ) ;
#13730 = AXIS2_PLACEMENT_3D ( 'NONE', #3109, #9064, #18832 ) ;
#13731 = LINE ( 'NONE', #5611, #7866 ) ;
#13732 = ORIENTED_EDGE ( 'NONE', *, *, #4712, .T. ) ;
#13733 = VERTEX_POINT ( 'NONE', #14859 ) ;
#13735 = ADVANCED_FACE ( 'NONE', ( #18737, #1069 ), #22596, .F. ) ;
#13734 = LINE ( 'NONE', #7430, #10184 ) ;
#13736 = CARTESIAN_POINT ( 'NONE',  ( 39.24876120206128860, -12.71368208888610241, 70.63227792289245599 ) ) ;
#13737 = ADVANCED_FACE ( 'NONE', ( #3265 ), #22849, .F. ) ;
#13738 = CARTESIAN_POINT ( 'NONE',  ( 39.31564783533280405, -12.31368208888610027, 72.03616607671141026 ) ) ;
#13739 = ORIENTED_EDGE ( 'NONE', *, *, #6264, .F. ) ;
#13740 = VECTOR ( 'NONE', #20146, 1000.000000000000114 ) ;
#13741 = EDGE_CURVE ( 'NONE', #8063, #12188, #18602, .T. ) ;
#13742 = VERTEX_POINT ( 'NONE', #21054 ) ;
#13743 = CARTESIAN_POINT ( 'NONE',  ( 43.06606138205700063, -34.55876147765400219, 74.30501292737011454 ) ) ;
#13744 = CYLINDRICAL_SURFACE ( 'NONE', #2148, 1.000000000000000888 ) ;
#13745 = ORIENTED_EDGE ( 'NONE', *, *, #15190, .T. ) ;
#13746 = DIRECTION ( 'NONE',  ( -1.000000000000000000, -1.052872940142565459E-15, -1.848188032574765003E-17 ) ) ;
#13747 = CARTESIAN_POINT ( 'NONE',  ( 37.69796330110505522, -18.50384086642191406, 73.09843995877329803 ) ) ;
#13748 = CARTESIAN_POINT ( 'NONE',  ( 36.57656417722905928, -21.26763587820238044, 75.85745157953545004 ) ) ;
#13749 = DIRECTION ( 'NONE',  ( -1.000000000000000000, 0.000000000000000000, 0.000000000000000000 ) ) ;
#13750 = CARTESIAN_POINT ( 'NONE',  ( 37.38336156205274818, -17.71368208888609885, 72.12822762946750288 ) ) ;
#13751 = ORIENTED_EDGE ( 'NONE', *, *, #16846, .F. ) ;
#13752 = AXIS2_PLACEMENT_3D ( 'NONE', #23176, #20876, #1651 ) ;
#13753 = ORIENTED_EDGE ( 'NONE', *, *, #25099, .F. ) ;
#13754 = FACE_OUTER_BOUND ( 'NONE', #12323, .T. ) ;
#13755 = CARTESIAN_POINT ( 'NONE',  ( 37.25202387243752611, -17.21368208888610241, 70.00779233799262613 ) ) ;
#13756 = EDGE_CURVE ( 'NONE', #22006, #1510, #6357, .T. ) ;
#13757 = AXIS2_PLACEMENT_3D ( 'NONE', #12961, #11018, #11404 ) ;
#13758 = CARTESIAN_POINT ( 'NONE',  ( 33.31606138205700773, -19.13113579875042802, 24.60350147050422720 ) ) ;
#13759 = DIRECTION ( 'NONE',  ( 0.000000000000000000, 0.000000000000000000, -1.000000000000000000 ) ) ;
#13760 = CARTESIAN_POINT ( 'NONE',  ( 39.29254315202756231, -28.81368208888610383, 69.94417936956671156 ) ) ;
#13761 = LINE ( 'NONE', #17751, #24190 ) ;
#13762 = CARTESIAN_POINT ( 'NONE',  ( 44.31606138205700063, -20.88462213365835041, 44.49284693532412405 ) ) ;
#13763 = ORIENTED_EDGE ( 'NONE', *, *, #1215, .F. ) ;
#13764 = PRESENTATION_LAYER_ASSIGNMENT (  '', '', ( #21575 ) ) ;
#13765 = LINE ( 'NONE', #23153, #15649 ) ;
#13766 = ORIENTED_EDGE ( 'NONE', *, *, #4768, .T. ) ;
#13767 = ORIENTED_EDGE ( 'NONE', *, *, #17059, .F. ) ;
#13768 = TOROIDAL_SURFACE ( 'NONE', #16618, 1.250000000000000000, 0.5000000000000000000 ) ;
#13769 = CARTESIAN_POINT ( 'NONE',  ( 36.98690846071097127, -5.803840866421911215, 69.45876917294177133 ) ) ;
#13770 = ORIENTED_EDGE ( 'NONE', *, *, #13988, .T. ) ;
#13771 = DIRECTION ( 'NONE',  ( 0.000000000000000000, 1.000000000000000000, 0.000000000000000000 ) ) ;
#13772 = CARTESIAN_POINT ( 'NONE',  ( 39.98359781491296161, -14.41368208888610525, 71.86517103874047052 ) ) ;
#13773 = FILL_AREA_STYLE_COLOUR ( '', #24403 ) ;
#13774 = VERTEX_POINT ( 'NONE', #24763 ) ;
#13775 = LINE ( 'NONE', #9667, #25305 ) ;
#13776 = CARTESIAN_POINT ( 'NONE',  ( 38.37017380507020192, -12.01368208888611022, 73.71602215082113219 ) ) ;
#13777 = ORIENTED_EDGE ( 'NONE', *, *, #24087, .T. ) ;
#13778 = CARTESIAN_POINT ( 'NONE',  ( 44.81606138205700063, -38.55876147765410167, 72.21586839016146087 ) ) ;
#13779 = FACE_OUTER_BOUND ( 'NONE', #14962, .T. ) ;
#13780 = ADVANCED_FACE ( 'NONE', ( #7010 ), #14996, .F. ) ;
#13781 = AXIS2_PLACEMENT_3D ( 'NONE', #17801, #23451, #5818 ) ;
#13782 = CARTESIAN_POINT ( 'NONE',  ( 33.31606138205700773, -29.06829118875199924, 75.30501292737000085 ) ) ;
#13783 = DIRECTION ( 'NONE',  ( 0.000000000000000000, -2.999999999999999839E-15, -1.000000000000000000 ) ) ;
#13784 = CARTESIAN_POINT ( 'NONE',  ( 37.89291511884479036, -10.50384086642191050, 72.49843995877331793 ) ) ;
#13785 = CARTESIAN_POINT ( 'NONE',  ( 39.41296390513587511, -28.41368208888610525, 71.67976084211548482 ) ) ;
#13786 = ORIENTED_EDGE ( 'NONE', *, *, #21302, .F. ) ;
#13787 = CARTESIAN_POINT ( 'NONE',  ( 40.05426416818898616, -21.26971791756611907, 75.85724679419259076 ) ) ;
#13788 = CARTESIAN_POINT ( 'NONE',  ( -3.287286993713738101E-16, 0.06621141594058931046, 0.03267658921011617340 ) ) ;
#13789 = ORIENTED_EDGE ( 'NONE', *, *, #11073, .T. ) ;
#13790 = EDGE_LOOP ( 'NONE', ( #14898, #25278, #1268, #15306 ) ) ;
#13791 = CARTESIAN_POINT ( 'NONE',  ( 36.89935272106205133, -28.40384086642191619, 73.23812341099225875 ) ) ;
#13792 = CARTESIAN_POINT ( 'NONE',  ( 39.24876120206128860, -22.71368208888610241, 70.63227792289245599 ) ) ;
#13793 = CARTESIAN_POINT ( 'NONE',  ( 39.73277004305198545, -0.2136820888861065970, 73.23812341099225875 ) ) ;
#13794 = ORIENTED_EDGE ( 'NONE', *, *, #18059, .T. ) ;
#13795 = CARTESIAN_POINT ( 'NONE',  ( 36.31606138205700063, -13.58280000135113674, 20.54174511886706256 ) ) ;
#13796 = CARTESIAN_POINT ( 'NONE',  ( 38.93987200065210175, 1.196159133578088118, 72.33091598616827866 ) ) ;
#13797 = DIRECTION ( 'NONE',  ( -1.000000000000000000, 7.144651197284802049E-31, 8.673617379884039170E-17 ) ) ;
#13798 = ORIENTED_EDGE ( 'NONE', *, *, #9367, .T. ) ;
#13799 = CARTESIAN_POINT ( 'NONE',  ( 43.81606138205700063, -37.98241563432385703, 69.85268917996594951 ) ) ;
#13800 = LINE ( 'NONE', #13675, #18265 ) ;
#13801 = CARTESIAN_POINT ( 'NONE',  ( 36.89935272106205133, -8.403840866421919742, 73.23812341099225875 ) ) ;
#13802 = DIRECTION ( 'NONE',  ( 1.000000000000000000, 0.000000000000000000, 0.000000000000000000 ) ) ;
#13803 = CARTESIAN_POINT ( 'NONE',  ( 41.81606138205697221, -2.443590368994772888, -5.798199789213649424 ) ) ;
#13804 = CARTESIAN_POINT ( 'NONE',  ( 38.37017380507020192, -14.01368208888610845, 73.11602215082116629 ) ) ;
#13805 = DIRECTION ( 'NONE',  ( -1.000000000000000000, 5.510910596163088391E-31, 1.836970198721029688E-16 ) ) ;
#13806 = EDGE_CURVE ( 'NONE', #19200, #2551, #5085, .T. ) ;
#13807 = CARTESIAN_POINT ( 'NONE',  ( 39.95015449827720744, -24.61368208888610454, 70.79240656858104330 ) ) ;
#13808 = CARTESIAN_POINT ( 'NONE',  ( 40.31606138205700773, 39.69123852234597649, 69.30501292736988717 ) ) ;
#13809 = CARTESIAN_POINT ( 'NONE',  ( 37.33957961208645315, 0.1961591335780908663, 69.94417936956673998 ) ) ;
#13810 = CARTESIAN_POINT ( 'NONE',  ( 43.06468080341912241, 3.415100481987967562, 6.350457055188933886 ) ) ;
#13811 = CARTESIAN_POINT ( 'NONE',  ( 40.14115730948191185, -18.51368208888610667, 71.32335560751960202 ) ) ;
#13812 = DIRECTION ( 'NONE',  ( 1.000000000000000000, 8.911169920151748851E-16, 3.114923731923493702E-16 ) ) ;
#13813 = CARTESIAN_POINT ( 'NONE',  ( 36.87297107704149823, -17.90384086642190908, 70.26145752964252722 ) ) ;
#13814 = ADVANCED_FACE ( 'NONE', ( #10762 ), #13073, .F. ) ;
#13815 = DIRECTION ( 'NONE',  ( -0.1733269559585509378, 0.000000000000000000, -0.9848643390529188135 ) ) ;
#13816 = EDGE_CURVE ( 'NONE', #16707, #11368, #18649, .T. ) ;
#13817 = CARTESIAN_POINT ( 'NONE',  ( 38.37017380507020192, -10.01368208888611022, 73.11602215082118050 ) ) ;
#13818 = ORIENTED_EDGE ( 'NONE', *, *, #13000, .T. ) ;
#13819 = CARTESIAN_POINT ( 'NONE',  ( 36.29569395875879678, -21.31368208888610027, 69.98269868914867686 ) ) ;
#13820 = ORIENTED_EDGE ( 'NONE', *, *, #25301, .T. ) ;
#13821 = LINE ( 'NONE', #25136, #1228 ) ;
#13822 = EDGE_CURVE ( 'NONE', #8986, #17509, #7266, .T. ) ;
#13823 = CARTESIAN_POINT ( 'NONE',  ( 45.81606138205707879, -39.99575152356564445, 63.13209164280871022 ) ) ;
#13824 = CARTESIAN_POINT ( 'NONE',  ( 37.31647492878124694, -20.30384086642190766, 72.03616607671141026 ) ) ;
#13825 = ADVANCED_FACE ( 'NONE', ( #4951 ), #13203, .T. ) ;
#13826 = EDGE_CURVE ( 'NONE', #6661, #21036, #18233, .T. ) ;
#13827 = EDGE_LOOP ( 'NONE', ( #8193, #18370, #5081, #9891 ) ) ;
#13828 = ORIENTED_EDGE ( 'NONE', *, *, #13684, .T. ) ;
#13829 = CARTESIAN_POINT ( 'NONE',  ( 31.81606138205700418, 35.95440708241085304, 62.30501292736990138 ) ) ;
#13830 = DIRECTION ( 'NONE',  ( -1.000000000000000000, -1.052872940142565459E-15, -1.848188032574765003E-17 ) ) ;
#13831 = SURFACE_SIDE_STYLE ('',( #14551 ) ) ;
#13832 = CARTESIAN_POINT ( 'NONE',  ( 40.55423172469004101, -29.20384086642191335, 70.70992431699446001 ) ) ;
#13833 = CARTESIAN_POINT ( 'NONE',  ( 40.81606138205700773, 37.44123852234599781, 75.30501292736990138 ) ) ;
#13834 = CARTESIAN_POINT ( 'NONE',  ( 39.02088643472237095, -2.913682088886100363, 69.02690120949094421 ) ) ;
#13835 = ADVANCED_FACE ( 'NONE', ( #12698 ), #20538, .T. ) ;
#13836 = PRODUCT_DEFINITION_SHAPE ( 'NONE', 'NONE',  #23307 ) ;
#13837 = DIRECTION ( 'NONE',  ( -4.789116818843729608E-32, 1.000000000000000000, -3.130104260698260371E-15 ) ) ;
#13838 = ADVANCED_FACE ( 'NONE', ( #6880 ), #12821, .F. ) ;
#13839 = EDGE_LOOP ( 'NONE', ( #3470, #6058, #8041, #18129 ) ) ;
#13840 = ORIENTED_EDGE ( 'NONE', *, *, #8402, .T. ) ;
#13841 = DIRECTION ( 'NONE',  ( 0.000000000000000000, -1.000000000000000000, 0.000000000000000000 ) ) ;
#13842 = CARTESIAN_POINT ( 'NONE',  ( 35.81606138205700063, -6.959910619544162458, 20.07251914782757751 ) ) ;
#13843 = CARTESIAN_POINT ( 'NONE',  ( 36.80608444377002542, -20.30384086642191832, 72.40698646996133903 ) ) ;
#13844 = SURFACE_STYLE_USAGE ( .BOTH. , #15894 ) ;
#13845 = FACE_OUTER_BOUND ( 'NONE', #13839, .T. ) ;
#13846 = VERTEX_POINT ( 'NONE', #13330 ) ;
#13847 = CARTESIAN_POINT ( 'NONE',  ( 46.81606138205696510, -2.780187754385526233, -4.367921789353634843 ) ) ;
#13848 = ADVANCED_FACE ( 'NONE', ( #5460 ), #9716, .T. ) ;
#13849 = CARTESIAN_POINT ( 'NONE',  ( 35.64099152588522657, -9.607181138187000258, 73.02501292736999972 ) ) ;
#13850 = ORIENTED_EDGE ( 'NONE', *, *, #4846, .F. ) ;
#13851 = CARTESIAN_POINT ( 'NONE',  ( 37.25260217561390874, -6.003840866421913169, 70.97781676520604321 ) ) ;
#13852 = DIRECTION ( 'NONE',  ( 0.000000000000000000, -1.000000000000000000, 3.491481338843135327E-15 ) ) ;
#13853 = ORIENTED_EDGE ( 'NONE', *, *, #3486, .F. ) ;
#13854 = FACE_OUTER_BOUND ( 'NONE', #7077, .T. ) ;
#13855 = ORIENTED_EDGE ( 'NONE', *, *, #4387, .F. ) ;
#13856 = EDGE_LOOP ( 'NONE', ( #7810, #12510, #585, #11487 ) ) ;
#13857 = PLANE ( 'NONE',  #1522 ) ;
#13858 = CARTESIAN_POINT ( 'NONE',  ( 37.69225076346193504, -13.81368208888610383, 72.33091598616826445 ) ) ;
#13859 = CARTESIAN_POINT ( 'NONE',  ( 39.41296390513587511, -8.413682088886101695, 71.67976084211552745 ) ) ;
#13860 = ORIENTED_EDGE ( 'NONE', *, *, #18715, .F. ) ;
#13861 = ORIENTED_EDGE ( 'NONE', *, *, #3254, .F. ) ;
#13862 = DIRECTION ( 'NONE',  ( 1.000000000000000000, 0.000000000000000000, 0.000000000000000000 ) ) ;
#13863 = CARTESIAN_POINT ( 'NONE',  ( 44.06606138205700063, 40.39281886181299797, 82.55501292736983032 ) ) ;
#13864 = ORIENTED_EDGE ( 'NONE', *, *, #24306, .F. ) ;
#13865 = PLANE ( 'NONE',  #454 ) ;
#13866 = CARTESIAN_POINT ( 'NONE',  ( 37.80618814713138676, -17.70384086642190979, 69.62690120949091011 ) ) ;
#13867 = CIRCLE ( 'NONE', #2729, 1.249999999999995115 ) ;
#13868 = AXIS2_PLACEMENT_3D ( 'NONE', #15224, #4015, #24085 ) ;
#13869 = VECTOR ( 'NONE', #936, 1000.000000000000000 ) ;
#13870 = CARTESIAN_POINT ( 'NONE',  ( 45.81606138205700063, -36.30035594811079847, 74.91924054225879104 ) ) ;
#13871 = DIRECTION ( 'NONE',  ( 1.000000000000000000, 2.999999999999999839E-15, 0.000000000000000000 ) ) ;
#13872 = CARTESIAN_POINT ( 'NONE',  ( 39.37952058850012804, -16.61368208888610098, 70.97781676520601479 ) ) ;
#13873 = ORIENTED_EDGE ( 'NONE', *, *, #11194, .T. ) ;
#13874 = VERTEX_POINT ( 'NONE', #13701 ) ;
#13875 =( BOUNDED_SURFACE ( )  B_SPLINE_SURFACE ( 3, 1, ( 
 ( #17721, #52 ),
 ( #20282, #1422 ),
 ( #18594, #6619 ),
 ( #22206, #7353 ) ),
 .UNSPECIFIED., .F., .F., .T. ) 
 B_SPLINE_SURFACE_WITH_KNOTS ( ( 4, 4 ),
 ( 2, 2 ),
 ( 0.000000000000000000, 1.000000000000000000 ),
 ( 0.000000000000000000, 1.000000000000000000 ),
 .UNSPECIFIED. ) 
 GEOMETRIC_REPRESENTATION_ITEM ( )  RATIONAL_B_SPLINE_SURFACE ( (
 ( 1.000000000000000000, 1.000000000000000000),
 ( 0.8047378541243649375, 0.8047378541243649375),
 ( 0.8047378541243649375, 0.8047378541243649375),
 ( 1.000000000000000000, 1.000000000000000000) ) ) 
 REPRESENTATION_ITEM ( '' )  SURFACE ( )  );
#13876 = CARTESIAN_POINT ( 'NONE',  ( 39.81746892067405952, 40.95934826813394380, 79.52109337493035923 ) ) ;
#13877 = CARTESIAN_POINT ( 'NONE',  ( 38.37017380507020192, -14.01368208888610845, 73.11602215082116629 ) ) ;
#13878 = DIRECTION ( 'NONE',  ( -3.469446951953614189E-15, 0.8967398287344635621, 0.4425581086832386379 ) ) ;
#13879 = EDGE_CURVE ( 'NONE', #20215, #7904, #7908, .T. ) ;
#13880 = LINE ( 'NONE', #4217, #13711 ) ;
#13881 = CARTESIAN_POINT ( 'NONE',  ( 43.31606138205700063, -21.26162886970023536, 44.16441745890789150 ) ) ;
#13882 = CARTESIAN_POINT ( 'NONE',  ( 40.08847615259004016, -29.10876147765399224, 71.39729523596237470 ) ) ;
#13883 = AXIS2_PLACEMENT_3D ( 'NONE', #13672, #17409, #15343 ) ;
#13884 = CARTESIAN_POINT ( 'NONE',  ( 38.31606138205700063, 38.69123852234599781, 71.30501292737000085 ) ) ;
#13885 = DIRECTION ( 'NONE',  ( -1.000000000000000000, -2.999999999999999839E-15, 0.000000000000000000 ) ) ;
#13886 = AXIS2_PLACEMENT_3D ( 'NONE', #8747, #6549, #12620 ) ;
#13887 = VERTEX_POINT ( 'NONE', #3908 ) ;
#13888 = FACE_OUTER_BOUND ( 'NONE', #16221, .T. ) ;
#13889 = ORIENTED_EDGE ( 'NONE', *, *, #8021, .T. ) ;
#13890 = ORIENTED_EDGE ( 'NONE', *, *, #19571, .F. ) ;
#13891 = CARTESIAN_POINT ( 'NONE',  ( 40.77203464402485622, -3.103840866421913258, 71.43714994484034264 ) ) ;
#13892 = ORIENTED_EDGE ( 'NONE', *, *, #13816, .T. ) ;
#13893 = CARTESIAN_POINT ( 'NONE',  ( 36.31606138205700063, -1.357181138186124736, 83.30501292736991559 ) ) ;
#13894 = CARTESIAN_POINT ( 'NONE',  ( 39.75915168707250302, -8.713682088886097077, 70.26145752964252722 ) ) ;
#13895 = VERTEX_POINT ( 'NONE', #15755 ) ;
#13896 = DIRECTION ( 'NONE',  ( 0.000000000000000000, -0.9841782327363374216, 0.1771812806364704285 ) ) ;
#13897 = CARTESIAN_POINT ( 'NONE',  ( 40.26954217208371034, -14.71368208888610241, 69.89063713639258424 ) ) ;
#13898 = VECTOR ( 'NONE', #21740, 1000.000000000000000 ) ;
#13899 = SURFACE_STYLE_USAGE ( .BOTH. , #1902 ) ;
#13900 = VECTOR ( 'NONE', #19248, 1000.000000000000000 ) ;
#13901 = VECTOR ( 'NONE', #5895, 1000.000000000000000 ) ;
#13902 = CARTESIAN_POINT ( 'NONE',  ( 43.31606138205700063, -13.25716901376041967, 21.21736665487721041 ) ) ;
#13903 = EDGE_CURVE ( 'NONE', #21773, #4055, #3422, .T. ) ;
#13904 = DIRECTION ( 'NONE',  ( 0.000000000000000000, 1.000000000000000000, 0.000000000000000000 ) ) ;
#13905 =( LENGTH_UNIT ( ) NAMED_UNIT ( * ) SI_UNIT ( .MILLI., .METRE. ) );
#13906 = EDGE_CURVE ( 'NONE', #9564, #12562, #23611, .T. ) ;
#13907 = LINE ( 'NONE', #4497, #23819 ) ;
#13908 = DIRECTION ( 'NONE',  ( 1.000000000000000000, 0.000000000000000000, 0.000000000000000000 ) ) ;
#13909 = LINE ( 'NONE', #741, #11919 ) ;
#13910 = CARTESIAN_POINT ( 'NONE',  ( 39.24876120206128860, -26.71368208888610596, 70.63227792289242757 ) ) ;
#13911 = ORIENTED_EDGE ( 'NONE', *, *, #22167, .T. ) ;
#13912 = CARTESIAN_POINT ( 'NONE',  ( 33.31606138205700773, -5.204193249396280585, 82.80501292736992980 ) ) ;
#13913 = DIRECTION ( 'NONE',  ( -5.047295537021760406E-31, 1.000000000000000000, -3.491481338843135327E-15 ) ) ;
#13914 = ORIENTED_EDGE ( 'NONE', *, *, #20700, .F. ) ;
#13915 = CIRCLE ( 'NONE', #6503, 1.000000000000000888 ) ;
#13916 = ORIENTED_EDGE ( 'NONE', *, *, #10450, .F. ) ;
#13917 = CARTESIAN_POINT ( 'NONE',  ( 35.86008812008917346, -24.10384086642191193, 71.32335560751960202 ) ) ;
#13918 = CIRCLE ( 'NONE', #2792, 0.7500000000000006661 ) ;
#13919 = AXIS2_PLACEMENT_3D ( 'NONE', #1091, #10779, #5112 ) ;
#13920 = EDGE_CURVE ( 'NONE', #19274, #20085, #5972, .T. ) ;
#13921 = CARTESIAN_POINT ( 'NONE',  ( 39.51027997493896748, -26.51368208888610667, 71.32335560751960202 ) ) ;
#13922 = CARTESIAN_POINT ( 'NONE',  ( 35.86008812008917346, 0.4863179111138961064, 71.43714994484035685 ) ) ;
#13923 = ORIENTED_EDGE ( 'NONE', *, *, #17754, .F. ) ;
#13924 = CARTESIAN_POINT ( 'NONE',  ( 38.48938833801555148, -33.30876147765400219, 72.28987726642316147 ) ) ;
#13925 = CARTESIAN_POINT ( 'NONE',  ( 39.37952058850012804, -1.003840866421912281, 71.78268878715392987 ) ) ;
#13926 = LINE ( 'NONE', #21782, #3603 ) ;
#13927 = ORIENTED_EDGE ( 'NONE', *, *, #8829, .T. ) ;
#13928 = PLANE ( 'NONE',  #6806 ) ;
#13929 = CARTESIAN_POINT ( 'NONE',  ( 45.81606138205707168, -36.31746077171914067, 73.86860304758450013 ) ) ;
#13930 = CARTESIAN_POINT ( 'NONE',  ( 40.52078840805429394, -3.003840866421914502, 72.15350918040385864 ) ) ;
#13931 = VECTOR ( 'NONE', #22856, 1000.000000000000227 ) ;
#13932 = DIRECTION ( 'NONE',  ( -1.000000000000000000, 0.000000000000000000, 0.000000000000000000 ) ) ;
#13933 =( NAMED_UNIT ( * ) SI_UNIT ( $, .STERADIAN. ) SOLID_ANGLE_UNIT ( ) );
#13934 = CARTESIAN_POINT ( 'NONE',  ( 37.69796330110504101, -5.113682088886101873, 69.66206559358663242 ) ) ;
#13935 = DIRECTION ( 'NONE',  ( 1.000000000000000000, 3.469446951953611033E-15, 0.000000000000000000 ) ) ;
#13936 = CARTESIAN_POINT ( 'NONE',  ( 38.93415946300898867, -26.11368208888610454, 73.09843995877328382 ) ) ;
#13937 = AXIS2_PLACEMENT_3D ( 'NONE', #22458, #13437, #7510 ) ;
#13938 = CARTESIAN_POINT ( 'NONE',  ( 36.31606138205700063, -13.25716901376042856, 21.21736665487721041 ) ) ;
#13939 = CARTESIAN_POINT ( 'NONE',  ( 39.82603832034401137, -3.303840866421908551, 70.35351908239860563 ) ) ;
#13940 = FACE_OUTER_BOUND ( 'NONE', #19367, .T. ) ;
#13941 = VECTOR ( 'NONE', #5168, 1000.000000000000000 ) ;
#13942 = CARTESIAN_POINT ( 'NONE',  ( 38.37017380507020192, -10.01368208888611022, 73.11602215082118050 ) ) ;
#13943 = DIRECTION ( 'NONE',  ( -1.000000000000000000, -6.197457809535974789E-17, -1.134781633102316229E-16 ) ) ;
#13944 = CARTESIAN_POINT ( 'NONE',  ( 38.26194895904384907, -12.60384086642191548, 73.11602215082116629 ) ) ;
#13945 = DIRECTION ( 'NONE',  ( -0.000000000000000000, 1.000000000000000000, -3.225463739888140187E-15 ) ) ;
#13946 = CARTESIAN_POINT ( 'NONE',  ( 38.93415946300897446, -14.11368208888610631, 73.09843995877329803 ) ) ;
#13947 = VERTEX_POINT ( 'NONE', #17567 ) ;
#13948 = CARTESIAN_POINT ( 'NONE',  ( 37.50301148336529167, -23.11368208888610454, 69.06206559358663810 ) ) ;
#13949 = ORIENTED_EDGE ( 'NONE', *, *, #2650, .F. ) ;
#13950 = CARTESIAN_POINT ( 'NONE',  ( 33.31606138205700773, 7.864187680719676443, 65.89022736311019912 ) ) ;
#13951 = DIRECTION ( 'NONE',  ( 1.000000000000000000, 2.999999999999999839E-15, 0.000000000000000000 ) ) ;
#13952 = CARTESIAN_POINT ( 'NONE',  ( 39.51027997493896748, -15.10384086642191370, 71.43714994484032843 ) ) ;
#13953 = VECTOR ( 'NONE', #8912, 1000.000000000000000 ) ;
#13954 = ORIENTED_EDGE ( 'NONE', *, *, #10837, .F. ) ;
#13955 = EDGE_LOOP ( 'NONE', ( #13987, #5395, #24658, #23942 ) ) ;
#13956 = CARTESIAN_POINT ( 'NONE',  ( 40.64099152588522657, -9.607181138187000258, 82.55501292736997243 ) ) ;
#13957 = FACE_OUTER_BOUND ( 'NONE', #23760, .T. ) ;
#13958 = CARTESIAN_POINT ( 'NONE',  ( 36.89935272106205133, -20.40384086642192329, 73.23812341099225875 ) ) ;
#13959 = CIRCLE ( 'NONE', #10679, 1.100000000000000311 ) ;
#13960 = CARTESIAN_POINT ( 'NONE',  ( 43.81606138205700063, -20.88462213363798270, 44.49284693533410717 ) ) ;
#13961 = CARTESIAN_POINT ( 'NONE',  ( 39.73277004305198545, -0.2136820888861065970, 73.23812341099225875 ) ) ;
#13962 = PLANE ( 'NONE',  #10207 ) ;
#13963 = ORIENTED_EDGE ( 'NONE', *, *, #1820, .F. ) ;
#13964 = VECTOR ( 'NONE', #4847, 1000.000000000000000 ) ;
#13965 = EDGE_CURVE ( 'NONE', #4719, #13410, #25395, .T. ) ;
#13966 = VERTEX_POINT ( 'NONE', #9595 ) ;
#13967 = CARTESIAN_POINT ( 'NONE',  ( 31.56606138205697576, -4.349482454670882348, -5.142398479549302515 ) ) ;
#13968 = EDGE_CURVE ( 'NONE', #2309, #5235, #14929, .T. ) ;
#13969 = DIRECTION ( 'NONE',  ( 0.000000000000000000, 2.775557561562888984E-15, 1.000000000000000000 ) ) ;
#13970 = CARTESIAN_POINT ( 'NONE',  ( 39.98359781491296161, -19.20384086642191335, 70.89533451361945993 ) ) ;
#13971 = EDGE_CURVE ( 'NONE', #8221, #18554, #1833, .T. ) ;
#13972 = DIRECTION ( 'NONE',  ( 1.000000000000000000, 0.000000000000000000, 0.000000000000000000 ) ) ;
#13973 = EDGE_CURVE ( 'NONE', #13207, #18741, #7652, .T. ) ;
#13974 = EDGE_CURVE ( 'NONE', #6791, #9087, #9466, .T. ) ;
#13975 = AXIS2_PLACEMENT_3D ( 'NONE', #15746, #13812, #18069 ) ;
#13976 = VERTEX_POINT ( 'NONE', #3519 ) ;
#13977 = CARTESIAN_POINT ( 'NONE',  ( 31.81606138205700418, -38.55876147765400219, 75.30501292737012875 ) ) ;
#13978 = DIRECTION ( 'NONE',  ( 0.000000000000000000, -0.8191520442889929088, -0.5735764363510444941 ) ) ;
#13979 = ORIENTED_EDGE ( 'NONE', *, *, #7364, .F. ) ;
#13980 = CARTESIAN_POINT ( 'NONE',  ( 39.02742774030101458, -5.403840866421909972, 70.49320253461759478 ) ) ;
#13981 = CIRCLE ( 'NONE', #12361, 3.000000000000000888 ) ;
#13982 = CARTESIAN_POINT ( 'NONE',  ( 30.81606138205700418, 40.39281886181299797, 66.30501292737000085 ) ) ;
#13983 = VERTEX_POINT ( 'NONE', #15493 ) ;
#13984 = EDGE_CURVE ( 'NONE', #4055, #21773, #13309, .T. ) ;
#13985 = DIRECTION ( 'NONE',  ( 0.000000000000000000, 0.7540134720837717852, 0.6568589528324747517 ) ) ;
#13986 = ORIENTED_EDGE ( 'NONE', *, *, #12178, .F. ) ;
#13987 = ORIENTED_EDGE ( 'NONE', *, *, #13243, .T. ) ;
#13988 = EDGE_CURVE ( 'NONE', #13325, #9870, #1461, .T. ) ;
#13989 = DIRECTION ( 'NONE',  ( 0.000000000000000000, 0.8212051873014208914, 0.5706330172266919076 ) ) ;
#13990 = VECTOR ( 'NONE', #9548, 1000.000000000000227 ) ;
#13991 = CARTESIAN_POINT ( 'NONE',  ( 37.25260217561390874, -7.613682088886100985, 71.78268878715394408 ) ) ;
#13992 = CARTESIAN_POINT ( 'NONE',  ( 37.31647492878122563, -5.313682088886097610, 70.72433947564853440 ) ) ;
#13993 = VERTEX_POINT ( 'NONE', #23475 ) ;
#13994 = VERTEX_POINT ( 'NONE', #5840 ) ;
#13995 = CARTESIAN_POINT ( 'NONE',  ( 40.31606138205697221, 33.19123852234596939, 66.30501292736991559 ) ) ;
#13996 = PLANE ( 'NONE',  #2567 ) ;
#13997 = LINE ( 'NONE', #21846, #18162 ) ;
#13998 = VECTOR ( 'NONE', #15974, 1000.000000000000000 ) ;
#13999 = CARTESIAN_POINT ( 'NONE',  ( 37.33957961208645315, -11.80384086642190944, 69.94417936956672577 ) ) ;
#14000 = CARTESIAN_POINT ( 'NONE',  ( 30.81606138205697931, -4.589472609077253296, -6.350807634294811876 ) ) ;
#14001 = B_SPLINE_CURVE_WITH_KNOTS ( 'NONE', 3,
 ( #24038, #8469, #10400, #11968, #83, #9900, #12344, #19935, #23911, #19805, #21614, #12213, #6526, #13882, #6025, #21992 ),
 .UNSPECIFIED., .F., .F.,
 ( 4, 2, 2, 2, 2, 2, 2, 4 ),
 ( 0.001207831664637873956, 0.001646106639017851266, 0.002084381613397828792, 0.002522656587777805885, 0.002741794074967794648, 0.002851362818562789246, 0.002906147190360304326, 0.002960931562157818973 ),
 .UNSPECIFIED. ) ;
#14002 = DIRECTION ( 'NONE',  ( 0.000000000000000000, 0.000000000000000000, -1.000000000000000000 ) ) ;
#14003 = CARTESIAN_POINT ( 'NONE',  ( 30.81606138205700418, -3.831401139557048197, 80.75501292737000369 ) ) ;
#14004 = ORIENTED_EDGE ( 'NONE', *, *, #17764, .T. ) ;
#14005 = ORIENTED_EDGE ( 'NONE', *, *, #2958, .F. ) ;
#14006 = CARTESIAN_POINT ( 'NONE',  ( 42.90907157547734840, 3.273800194541344855, 6.355715097684958792 ) ) ;
#14007 = AXIS2_PLACEMENT_3D ( 'NONE', #3739, #15724, #15211 ) ;
#14008 = CARTESIAN_POINT ( 'NONE',  ( 38.93415946300898867, -16.11368208888611164, 73.09843995877329803 ) ) ;
#14009 = LINE ( 'NONE', #21862, #13498 ) ;
#14010 = CARTESIAN_POINT ( 'NONE',  ( 38.31606138205700063, 39.69123852234598360, 71.30501292737018559 ) ) ;
#14011 = ADVANCED_FACE ( 'NONE', ( #19235 ), #1573, .T. ) ;
#14012 = PLANE ( 'NONE',  #3668 ) ;
#14013 = CARTESIAN_POINT ( 'NONE',  ( 45.81606138205700063, -36.05876147765410877, 70.30501292737000085 ) ) ;
#14014 = CARTESIAN_POINT ( 'NONE',  ( 38.31606138205700063, -29.37462871496113337, 53.20604314849776983 ) ) ;
#14015 = DIRECTION ( 'NONE',  ( -1.000000000000000000, -2.999999999999999839E-15, 0.000000000000000000 ) ) ;
#14016 = ORIENTED_EDGE ( 'NONE', *, *, #15066, .T. ) ;
#14017 = CARTESIAN_POINT ( 'NONE',  ( 43.81606138205700063, 41.44123852234596939, 66.30501292736988717 ) ) ;
#14018 = ORIENTED_EDGE ( 'NONE', *, *, #4765, .T. ) ;
#14019 = VERTEX_POINT ( 'NONE', #9839 ) ;
#14020 = CARTESIAN_POINT ( 'NONE',  ( 33.31606138205700773, -39.23120981750657421, 69.49370132789680099 ) ) ;
#14021 = CARTESIAN_POINT ( 'NONE',  ( 35.86008812008917346, -4.103840866421913702, 71.32335560751961623 ) ) ;
#14022 = CIRCLE ( 'NONE', #15668, 2.000000000000001776 ) ;
#14023 = ORIENTED_EDGE ( 'NONE', *, *, #23804, .T. ) ;
#14024 = LINE ( 'NONE', #3972, #4608 ) ;
#14025 = CARTESIAN_POINT ( 'NONE',  ( 39.95015449827720744, -6.613682088886106314, 70.79240656858107172 ) ) ;
#14026 = AXIS2_PLACEMENT_3D ( 'NONE', #4259, #2301, #18042 ) ;
#14027 = VERTEX_POINT ( 'NONE', #17696 ) ;
#14028 = CARTESIAN_POINT ( 'NONE',  ( 40.56606138205700773, 5.594015759443068170, 2.006005027196319901 ) ) ;
#14029 = EDGE_CURVE ( 'NONE', #24723, #22752, #7121, .T. ) ;
#14030 = CARTESIAN_POINT ( 'NONE',  ( 37.50301148336529167, -13.11368208888610454, 69.06206559358665231 ) ) ;
#14031 = CARTESIAN_POINT ( 'NONE',  ( 39.31606138205702194, -20.92507021039839543, 32.39841118875936132 ) ) ;
#14032 = CARTESIAN_POINT ( 'NONE',  ( 31.81606138205700418, 41.44123852234599070, 73.55501292736987295 ) ) ;
#14033 = LINE ( 'NONE', #17909, #15317 ) ;
#14034 = PRESENTATION_STYLE_ASSIGNMENT (( #5660 ) ) ;
#14035 = LINE ( 'NONE', #14169, #21775 ) ;
#14036 = CARTESIAN_POINT ( 'NONE',  ( 38.31606138205700063, -7.086900875803856970, 56.51273394326043586 ) ) ;
#14037 = AXIS2_PLACEMENT_3D ( 'NONE', #15785, #16278, #10369 ) ;
#14038 = DIRECTION ( 'NONE',  ( -1.000000000000000000, 0.000000000000000000, 0.000000000000000000 ) ) ;
#14039 = CARTESIAN_POINT ( 'NONE',  ( 39.41296390513587511, -26.41368208888610170, 71.67976084211548482 ) ) ;
#14040 = EDGE_LOOP ( 'NONE', ( #22994, #5360, #6035, #899 ) ) ;
#14041 = CARTESIAN_POINT ( 'NONE',  ( 39.53940869104339839, -21.82971330735793813, 75.81783783739737714 ) ) ;
#14042 = PLANE ( 'NONE',  #14026 ) ;
#14043 = ORIENTED_EDGE ( 'NONE', *, *, #14152, .F. ) ;
#14044 = ORIENTED_EDGE ( 'NONE', *, *, #5298, .F. ) ;
#14045 = CARTESIAN_POINT ( 'NONE',  ( 38.26194895904384197, -24.60384086642191903, 73.71602215082113219 ) ) ;
#14046 = B_SPLINE_SURFACE_WITH_KNOTS ( 'NONE', 1, 3, ( 
 ( #12502, #10555, #6810, #18530, #740, #8622, #16459, #14790, #4873, #8882, #20589, #24689, #24305, #2922, #16720, #24554, #6935, #14912 ),
 ( #22649, #12868, #20723, #22774, #3059, #10935, #18783, #1501, #15427, #15295, #23146, #5635, #13124, #13499, #7446, #17501, #11450, #5519 ),
 ( #23276, #7584, #13628, #25192, #23022, #17116, #21349, #19288, #3696, #19412, #11578, #19165, #24932, #17362, #1753, #7320, #25325, #5387 ),
 ( #9651, #1625, #9270, #20980, #13253, #7703, #5768, #15549, #21229, #9390, #3451, #3563, #13384, #3320, #21480, #23397, #21105, #9520 ) ),
 .UNSPECIFIED., .F., .F., .F.,
 ( 2, 1, 1, 2 ),
 ( 4, 2, 2, 2, 2, 2, 2, 2, 4 ),
 ( -0.01000000000000000021, 0.000000000000000000, 1.000000000000000000, 1.010099999999999998 ),
 ( 0.000000000000000000, 0.0003923663566484079674, 0.0007847327132968159348, 0.001177099069945223902, 0.001569465426593629918, 0.001961831783242040054, 0.002354198139890449973, 0.002746564496538855121, 0.003138930853187265040 ),
 .UNSPECIFIED. ) ;
#14047 = CARTESIAN_POINT ( 'NONE',  ( 38.93415946300897446, -26.11368208888610098, 73.09843995877328382 ) ) ;
#14048 = PLANE ( 'NONE',  #10323 ) ;
#14049 = ADVANCED_FACE ( 'NONE', ( #7524 ), #15372, .T. ) ;
#14050 = EDGE_CURVE ( 'NONE', #2401, #13623, #25204, .T. ) ;
#14051 = PLANE ( 'NONE',  #12678 ) ;
#14052 = VERTEX_POINT ( 'NONE', #21935 ) ;
#14053 = CARTESIAN_POINT ( 'NONE',  ( 39.62251006394166097, -5.661281603007885188, 82.79494754200436546 ) ) ;
#14054 = ADVANCED_FACE ( 'NONE', ( #20001 ), #8037, .T. ) ;
#14055 = DIRECTION ( 'NONE',  ( 0.000000000000000000, -0.5706330172266896872, 0.8212051873014225567 ) ) ;
#14056 = CARTESIAN_POINT ( 'NONE',  ( 36.11133435605973574, -4.003840866421914946, 70.60699637195612866 ) ) ;
#14057 = FACE_OUTER_BOUND ( 'NONE', #14329, .T. ) ;
#14058 = CARTESIAN_POINT ( 'NONE',  ( 33.23377536606392368, 3.110316458148107976, 6.136481421541682302 ) ) ;
#14059 = CARTESIAN_POINT ( 'NONE',  ( 36.87297107704152666, -7.713682088886109511, 72.49904802271743165 ) ) ;
#14060 = DIRECTION ( 'NONE',  ( 1.000000000000000000, 0.000000000000000000, 0.000000000000000000 ) ) ;
#14061 = CIRCLE ( 'NONE', #4613, 2.000000000000001776 ) ;
#14062 = CARTESIAN_POINT ( 'NONE',  ( 39.98359781491296161, -26.41368208888610525, 71.86517103874045631 ) ) ;
#14063 = DIRECTION ( 'NONE',  ( 1.225631768639319301E-15, -0.4425581086832399147, 0.8967398287344627850 ) ) ;
#14064 = EDGE_CURVE ( 'NONE', #2758, #24942, #2220, .T. ) ;
#14065 = CARTESIAN_POINT ( 'NONE',  ( 38.93415946300897446, 0.4961591335780924927, 69.66206559358666084 ) ) ;
#14066 = CARTESIAN_POINT ( 'NONE',  ( 33.66606138205698073, -6.672912525257909344, -0.4345143786933236552 ) ) ;
#14067 =( BOUNDED_CURVE ( )  B_SPLINE_CURVE ( 3, ( #2250, #309, #10124, #8188 ),
 .UNSPECIFIED., .F., .T. ) 
 B_SPLINE_CURVE_WITH_KNOTS ( ( 4, 4 ),
 ( 0.000000000000000000, 1.570796326794895004 ),
 .UNSPECIFIED. ) 
 CURVE ( )  GEOMETRIC_REPRESENTATION_ITEM ( )  RATIONAL_B_SPLINE_CURVE ( ( 1.000000000000000000, 0.8047378541243649375, 0.8047378541243649375, 1.000000000000000000 ) ) 
 REPRESENTATION_ITEM ( '' )  );
#14068 = CARTESIAN_POINT ( 'NONE',  ( 39.37952058850012804, -25.00384086642191406, 71.78268878715390144 ) ) ;
#14069 = CARTESIAN_POINT ( 'NONE',  ( 37.80618814713140097, -11.91368208888611058, 73.13360434286903455 ) ) ;
#14070 = DIRECTION ( 'NONE',  ( 0.000000000000000000, 3.469446951953611033E-15, 1.000000000000000000 ) ) ;
#14071 = VECTOR ( 'NONE', #18522, 1000.000000000000000 ) ;
#14072 = VECTOR ( 'NONE', #18024, 1000.000000000000000 ) ;
#14073 = CARTESIAN_POINT ( 'NONE',  ( 37.33957961208645315, -13.80384086642190766, 69.94417936956672577 ) ) ;
#14074 = DIRECTION ( 'NONE',  ( 1.000000000000000000, 1.734723475976804876E-16, -1.734723475976814737E-16 ) ) ;
#14075 = AXIS2_PLACEMENT_3D ( 'NONE', #14811, #9163, #12896 ) ;
#14076 = CARTESIAN_POINT ( 'NONE',  ( 38.37017380507020192, -12.01368208888610845, 73.11602215082116629 ) ) ;
#14077 = ORIENTED_EDGE ( 'NONE', *, *, #19086, .T. ) ;
#14078 = CARTESIAN_POINT ( 'NONE',  ( 36.89935272106204422, -15.21368208888610063, 69.52238214136768590 ) ) ;
#14079 = ORIENTED_EDGE ( 'NONE', *, *, #11311, .F. ) ;
#14080 = LINE ( 'NONE', #23978, #5361 ) ;
#14081 = DIRECTION ( 'NONE',  ( -2.122643018205887308E-17, 1.000000000000000000, -3.120611096041553009E-15 ) ) ;
#14082 = CARTESIAN_POINT ( 'NONE',  ( 39.37952058850012804, -21.00384086642191050, 71.78268878715390144 ) ) ;
#14083 = VERTEX_POINT ( 'NONE', #2592 ) ;
#14084 = ORIENTED_EDGE ( 'NONE', *, *, #18763, .T. ) ;
#14085 = DIRECTION ( 'NONE',  ( 2.727049986597864201E-15, -0.7516416929448760387, -0.6595716529892418079 ) ) ;
#14086 = DIRECTION ( 'NONE',  ( -1.000000000000000000, -1.000000000000000078E-15, 0.000000000000000000 ) ) ;
#14087 = CARTESIAN_POINT ( 'NONE',  ( 40.52078840805429394, -21.00384086642191761, 72.15350918040381600 ) ) ;
#14088 = LINE ( 'NONE', #23987, #4305 ) ;
#14089 = CARTESIAN_POINT ( 'NONE',  ( 37.33957961208646736, -23.81368208888611093, 72.81632618279320468 ) ) ;
#14090 = DIRECTION ( 'NONE',  ( 1.734723475976739795E-16, 4.343580702399009298E-14, 1.000000000000000000 ) ) ;
#14091 = AXIS2_PLACEMENT_3D ( 'NONE', #15040, #23020, #2798 ) ;
#14092 = VERTEX_POINT ( 'NONE', #21808 ) ;
#14093 = DIRECTION ( 'NONE',  ( 0.000000000000000000, 0.7540134720837717852, 0.6568589528324746407 ) ) ;
#14094 = LINE ( 'NONE', #18219, #3568 ) ;
#14095 = EDGE_CURVE ( 'NONE', #10641, #3863, #19058, .T. ) ;
#14096 = AXIS2_PLACEMENT_3D ( 'NONE', #983, #19155, #8871 ) ;
#14097 = CARTESIAN_POINT ( 'NONE',  ( 37.69796330110505522, -22.50384086642191406, 73.09843995877329803 ) ) ;
#14098 = SURFACE_STYLE_USAGE ( .BOTH. , #20020 ) ;
#14099 = DIRECTION ( 'NONE',  ( 1.000000000000000000, 2.168404344971050037E-16, -1.734723475976814737E-16 ) ) ;
#14100 = EDGE_LOOP ( 'NONE', ( #23407, #11256, #21513, #1459 ) ) ;
#14101 = DIRECTION ( 'NONE',  ( 2.727049986597864201E-15, -0.7516416929448760387, -0.6595716529892418079 ) ) ;
#14102 = AXIS2_PLACEMENT_3D ( 'NONE', #7058, #3315, #736 ) ;
#14103 = AXIS2_PLACEMENT_3D ( 'NONE', #18152, #17770, #23680 ) ;
#14104 = FACE_OUTER_BOUND ( 'NONE', #13160, .T. ) ;
#14105 = CARTESIAN_POINT ( 'NONE',  ( 39.38009889167648936, -29.40384086642190908, 70.00779233799262613 ) ) ;
#14106 = CARTESIAN_POINT ( 'NONE',  ( 40.31606138205700773, -18.80550481115971095, 25.27912300651437150 ) ) ;
#14107 = EDGE_LOOP ( 'NONE', ( #1614, #17344, #18571, #8699 ) ) ;
#14108 = DIRECTION ( 'NONE',  ( -1.000000000000000000, 1.115179377413661005E-30, 3.717264591378870232E-16 ) ) ;
#14109 = ORIENTED_EDGE ( 'NONE', *, *, #13519, .T. ) ;
#14110 = EDGE_LOOP ( 'NONE', ( #8959, #25300, #23341, #21082 ) ) ;
#14111 = CARTESIAN_POINT ( 'NONE',  ( 43.81606138205700063, 22.19123852234699967, 69.30501292736994401 ) ) ;
#14112 = VECTOR ( 'NONE', #17884, 1000.000000000000000 ) ;
#14113 = FACE_OUTER_BOUND ( 'NONE', #8473, .T. ) ;
#14114 = CARTESIAN_POINT ( 'NONE',  ( 39.02742774030102879, -8.213682088886098853, 72.26730301774236409 ) ) ;
#14115 = ADVANCED_FACE ( 'NONE', ( #20254 ), #4419, .T. ) ;
#14116 = ADVANCED_FACE ( 'NONE', ( #12035 ), #6358, .T. ) ;
#14117 = CARTESIAN_POINT ( 'NONE',  ( 38.37017380507020192, -4.013682088886100452, 72.51602215082118619 ) ) ;
#14118 = ORIENTED_EDGE ( 'NONE', *, *, #13126, .F. ) ;
#14119 = EDGE_LOOP ( 'NONE', ( #17506, #17598, #11686, #2135 ) ) ;
#14120 = DIRECTION ( 'NONE',  ( 1.000000000000000000, 1.288820809889844211E-16, 6.101052743105423043E-17 ) ) ;
#14121 = CIRCLE ( 'NONE', #2581, 3.999999999999899636 ) ;
#14122 = DIRECTION ( 'NONE',  ( 0.000000000000000000, 0.4425581086832400257, -0.8967398287344627850 ) ) ;
#14123 = ORIENTED_EDGE ( 'NONE', *, *, #1189, .F. ) ;
#14124 = DIRECTION ( 'NONE',  ( 0.000000000000000000, -0.7516416929448760387, -0.6595716529892418079 ) ) ;
#14125 = CARTESIAN_POINT ( 'NONE',  ( 37.80618814713138676, -9.703840866421904465, 69.62690120949091011 ) ) ;
#14126 = EDGE_CURVE ( 'NONE', #2216, #20225, #656, .T. ) ;
#14127 = DIRECTION ( 'NONE',  ( 0.000000000000000000, 0.5706330172266919076, -0.8212051873014208914 ) ) ;
#14128 = AXIS2_PLACEMENT_3D ( 'NONE', #18621, #16553, #1086 ) ;
#14129 = CARTESIAN_POINT ( 'NONE',  ( 40.31606138205700773, 38.69123852234599070, 73.55501292736988717 ) ) ;
#14130 = VERTEX_POINT ( 'NONE', #22184 ) ;
#14131 = VERTEX_POINT ( 'NONE', #24101 ) ;
#14132 = EDGE_LOOP ( 'NONE', ( #6037, #7203, #5872, #13020 ) ) ;
#14133 = DIRECTION ( 'NONE',  ( -1.000000000000000000, 0.000000000000000000, 0.000000000000000000 ) ) ;
#14134 = CARTESIAN_POINT ( 'NONE',  ( 38.37017380507020192, -8.013682088886108446, 73.11602215082118050 ) ) ;
#14135 = EDGE_CURVE ( 'NONE', #22793, #25358, #13709, .T. ) ;
#14136 = DIRECTION ( 'NONE',  ( -1.000000000000000000, -2.168404344971010101E-16, 1.734723475976814737E-16 ) ) ;
#14137 = AXIS2_PLACEMENT_3D ( 'NONE', #20150, #2485, #297 ) ;
#14138 = LINE ( 'NONE', #15927, #14112 ) ;
#14139 = CARTESIAN_POINT ( 'NONE',  ( 32.81606138205700773, 28.69846577177642288, 66.12638289304319983 ) ) ;
#14140 = LINE ( 'NONE', #12089, #12294 ) ;
#14141 = VECTOR ( 'NONE', #23953, 1000.000000000000000 ) ;
#14142 = DIRECTION ( 'NONE',  ( -1.734723475976804876E-16, 0.8212051873014210024, 0.5706330172266920187 ) ) ;
#14143 = DIRECTION ( 'NONE',  ( -1.000000000000000000, 6.018531076210130433E-31, 1.734723475976804876E-16 ) ) ;
#14144 = CIRCLE ( 'NONE', #21129, 0.2000000000000057288 ) ;
#14145 = CARTESIAN_POINT ( 'NONE',  ( 38.04888786834955994, -22.22120570019677288, 75.30501292736998664 ) ) ;
#14146 = ORIENTED_EDGE ( 'NONE', *, *, #11474, .F. ) ;
#14147 = ORIENTED_EDGE ( 'NONE', *, *, #11030, .F. ) ;
#14148 = CARTESIAN_POINT ( 'NONE',  ( 45.81606138205700063, -34.55876147765410167, 70.30501292737000085 ) ) ;
#14149 = CARTESIAN_POINT ( 'NONE',  ( 40.77203464402485622, -5.103840866421915479, 71.43714994484034264 ) ) ;
#14150 = EDGE_CURVE ( 'NONE', #21235, #8218, #20128, .T. ) ;
#14151 = PRESENTATION_LAYER_ASSIGNMENT (  '', '', ( #5078 ) ) ;
#14152 = EDGE_CURVE ( 'NONE', #21826, #17636, #17834, .T. ) ;
#14153 = ORIENTED_EDGE ( 'NONE', *, *, #3089, .T. ) ;
#14154 = LINE ( 'NONE', #343, #71 ) ;
#14155 = CARTESIAN_POINT ( 'NONE',  ( 37.80618814713140097, -5.913682088886107024, 73.13360434286904876 ) ) ;
#14156 = ADVANCED_FACE ( 'NONE', ( #23979, #532, #8417, #6474 ), #2088, .F. ) ;
#14157 = AXIS2_PLACEMENT_3D ( 'NONE', #22676, #24207, #10840 ) ;
#14158 = EDGE_CURVE ( 'NONE', #5343, #24841, #18332, .T. ) ;
#14159 = EDGE_CURVE ( 'NONE', #8450, #180, #23730, .T. ) ;
#14160 = DIRECTION ( 'NONE',  ( -1.000000000000000000, 0.000000000000000000, 0.000000000000000000 ) ) ;
#14161 = AXIS2_PLACEMENT_3D ( 'NONE', #8331, #12461, #14499 ) ;
#14162 = CARTESIAN_POINT ( 'NONE',  ( 40.26954217208371034, -16.71368208888610241, 69.89063713639258424 ) ) ;
#14163 = CARTESIAN_POINT ( 'NONE',  ( 43.05893253799167297, 3.408563886988916103, 6.350990360017464198 ) ) ;
#14164 = DIRECTION ( 'NONE',  ( 9.999999999999998805E-16, -0.9439899321577399638, -0.3299742535180969494 ) ) ;
#14165 = VERTEX_POINT ( 'NONE', #9969 ) ;
#14166 = DIRECTION ( 'NONE',  ( -1.734723475976804876E-16, -3.469446951953610245E-15, -1.000000000000000000 ) ) ;
#14167 = SURFACE_STYLE_FILL_AREA ( #24783 ) ;
#14168 = PRESENTATION_LAYER_ASSIGNMENT (  '', '', ( #16209 ) ) ;
#14169 = CARTESIAN_POINT ( 'NONE',  ( 32.31606138205700063, -20.55619265724211076, 44.11584019928223910 ) ) ;
#14170 = AXIS2_PLACEMENT_3D ( 'NONE', #22874, #16827, #18889 ) ;
#14171 = DIRECTION ( 'NONE',  ( 1.000000000000000000, -0.000000000000000000, 0.000000000000000000 ) ) ;
#14172 = DIRECTION ( 'NONE',  ( 1.000000000000000000, 0.000000000000000000, 0.000000000000000000 ) ) ;
#14173 = CARTESIAN_POINT ( 'NONE',  ( 37.60469502381300089, -23.21368208888610241, 70.49320253461758057 ) ) ;
#14174 = ORIENTED_EDGE ( 'NONE', *, *, #19634, .T. ) ;
#14175 = CARTESIAN_POINT ( 'NONE',  ( 40.31606138205700773, -20.22127907754186893, 75.50705395623725735 ) ) ;
#14176 = ADVANCED_FACE ( 'NONE', ( #6223 ), #17828, .T. ) ;
#14177 = VECTOR ( 'NONE', #8681, 1000.000000000000000 ) ;
#14178 = PLANE ( 'NONE',  #14818 ) ;
#14179 = ORIENTED_EDGE ( 'NONE', *, *, #8493, .T. ) ;
#14180 = VERTEX_POINT ( 'NONE', #10601 ) ;
#14181 = PRODUCT_DEFINITION_CONTEXT ( 'detailed design', #396, 'design' ) ;
#14182 = CARTESIAN_POINT ( 'NONE',  ( 40.77203464402485622, -25.10384086642191903, 71.43714994484031422 ) ) ;
#14183 = CARTESIAN_POINT ( 'NONE',  ( 38.26194895904383486, -25.01368208888610312, 69.64448340153876416 ) ) ;
#14184 = CARTESIAN_POINT ( 'NONE',  ( 36.31606138205700063, -13.58280000135113674, 20.54174511886706256 ) ) ;
#14185 = DIRECTION ( 'NONE',  ( -9.027796614315171564E-31, -1.000000000000000000, -3.938893903907230117E-15 ) ) ;
#14186 = ORIENTED_EDGE ( 'NONE', *, *, #20104, .T. ) ;
#14187 = CARTESIAN_POINT ( 'NONE',  ( 39.30543087153672843, -5.448589505030816404, 82.80225421346835901 ) ) ;
#14188 = LINE ( 'NONE', #19981, #14141 ) ;
#14189 = CARTESIAN_POINT ( 'NONE',  ( 36.36258059203030513, -5.903840866421909972, 69.89063713639259845 ) ) ;
#14190 = VECTOR ( 'NONE', #11369, 1000.000000000000000 ) ;
#14191 = FACE_OUTER_BOUND ( 'NONE', #2661, .T. ) ;
#14192 = CARTESIAN_POINT ( 'NONE',  ( 32.81606138205700773, 44.92314894770294131, 80.37823623207322044 ) ) ;
#14193 = CARTESIAN_POINT ( 'NONE',  ( 36.64852494920107517, -9.413682088886107024, 70.89533451361948835 ) ) ;
#14194 = CARTESIAN_POINT ( 'NONE',  ( 28.84183937708599998, -34.55876147765400219, 70.30501292737000085 ) ) ;
#14195 = CARTESIAN_POINT ( 'NONE',  ( 36.87297107704153376, -23.71368208888610596, 72.49904802271738902 ) ) ;
#14196 = VECTOR ( 'NONE', #1052, 1000.000000000000114 ) ;
#14197 = DIRECTION ( 'NONE',  ( -1.000000000000000000, 0.000000000000000000, 0.000000000000000000 ) ) ;
#14198 = CARTESIAN_POINT ( 'NONE',  ( 39.29254315202757653, 1.196159133578084788, 72.81632618279324731 ) ) ;
#14199 = ITEM_DEFINED_TRANSFORMATION ( 'NONE', 'NONE', #10471,  #2000 ) ;
#14200 = EDGE_CURVE ( 'NONE', #18480, #14416, #24832, .T. ) ;
#14201 = CARTESIAN_POINT ( 'NONE',  ( 43.09178375111335413, 3.447594731875835983, 6.345965694596597650 ) ) ;
#14202 = CARTESIAN_POINT ( 'NONE',  ( 39.41296390513587511, -25.20384086642191335, 71.08074471024438878 ) ) ;
#14203 = CARTESIAN_POINT ( 'NONE',  ( 38.82593461698262871, -12.91368208888610347, 69.62690120949091011 ) ) ;
#14204 = ADVANCED_FACE ( 'NONE', ( #24946 ), #15179, .F. ) ;
#14205 = PLANE ( 'NONE',  #2425 ) ;
#14206 = AXIS2_PLACEMENT_3D ( 'NONE', #3467, #3845, #23289 ) ;
#14207 = CARTESIAN_POINT ( 'NONE',  ( 38.82593461698265003, -14.70384086642191512, 73.13360434286903455 ) ) ;
#14208 = AXIS2_PLACEMENT_3D ( 'NONE', #9447, #9701, #17420 ) ;
#14209 = LINE ( 'NONE', #1950, #10577 ) ;
#14210 = CARTESIAN_POINT ( 'NONE',  ( 39.82603832034400426, -14.31368208888610916, 72.40698646996133903 ) ) ;
#14211 = VERTEX_POINT ( 'NONE', #22908 ) ;
#14212 = CARTESIAN_POINT ( 'NONE',  ( 40.33642880535524000, -16.31368208888611093, 72.77780686321126780 ) ) ;
#14213 = VERTEX_POINT ( 'NONE', #11338 ) ;
#14214 = CARTESIAN_POINT ( 'NONE',  ( 42.96606138205694236, 6.105630034208211931, 5.871938670042847974 ) ) ;
#14215 = DIRECTION ( 'NONE',  ( 0.000000000000000000, 0.7540134720837716742, 0.6568589528324746407 ) ) ;
#14216 = CARTESIAN_POINT ( 'NONE',  ( 39.24876120206129571, -18.90384086642191264, 72.12822762946747446 ) ) ;
#14217 = EDGE_LOOP ( 'NONE', ( #3844, #6241, #815, #17508 ) ) ;
#14218 = ORIENTED_EDGE ( 'NONE', *, *, #1395, .F. ) ;
#14219 = DIRECTION ( 'NONE',  ( 3.373073425510455500E-16, 2.999999999999999839E-15, 1.000000000000000000 ) ) ;
#14220 = ADVANCED_FACE ( 'NONE', ( #2840 ), #16998, .F. ) ;
#14221 = DIRECTION ( 'NONE',  ( 0.000000000000000000, -1.000000000000000000, 2.999999999999999839E-15 ) ) ;
#14222 = CARTESIAN_POINT ( 'NONE',  ( 39.64521430340305841, -22.80384086642191832, 73.30173637941818754 ) ) ;
#14223 = CARTESIAN_POINT ( 'NONE',  ( 32.81606138205700773, -33.60910547091194900, 60.61426200347987248 ) ) ;
#14224 = CARTESIAN_POINT ( 'NONE',  ( 36.68196826583682935, -27.61368208888610809, 71.96809898377887293 ) ) ;
#14225 = LINE ( 'NONE', #2479, #21715 ) ;
#14226 = VERTEX_POINT ( 'NONE', #16504 ) ;
#14227 = DIRECTION ( 'NONE',  ( 1.000000000000000000, -9.027796614315171564E-31, -4.436993566807132493E-46 ) ) ;
#14228 = CARTESIAN_POINT ( 'NONE',  ( 44.81606138205700063, 35.95440708241085304, 61.30501292736990138 ) ) ;
#14229 = CARTESIAN_POINT ( 'NONE',  ( 39.29254315202757653, -14.80384086642191477, 72.81632618279321889 ) ) ;
#14230 = EDGE_CURVE ( 'NONE', #6270, #7648, #1402, .T. ) ;
#14231 = CARTESIAN_POINT ( 'NONE',  ( 41.31606138205700063, 3.099306811489555891, 65.29760936252343129 ) ) ;
#14232 = EDGE_CURVE ( 'NONE', #19839, #11138, #295, .T. ) ;
#14233 = CARTESIAN_POINT ( 'NONE',  ( 38.31606138205700773, -21.82678658219787948, 29.70634659473178019 ) ) ;
#14234 = DIRECTION ( 'NONE',  ( -1.000000000000000000, 0.000000000000000000, 0.000000000000000000 ) ) ;
#14235 = CARTESIAN_POINT ( 'NONE',  ( 37.60469502381300799, -0.4038408664219124145, 72.26730301774236409 ) ) ;
#14236 = DIRECTION ( 'NONE',  ( -3.373073425510455500E-16, -2.999999999999999839E-15, -1.000000000000000000 ) ) ;
#14237 = ORIENTED_EDGE ( 'NONE', *, *, #25318, .F. ) ;
#14238 = LINE ( 'NONE', #22082, #24700 ) ;
#14239 = ORIENTED_EDGE ( 'NONE', *, *, #19349, .F. ) ;
#14240 = ORIENTED_EDGE ( 'NONE', *, *, #10827, .F. ) ;
#14241 = FACE_OUTER_BOUND ( 'NONE', #9397, .T. ) ;
#14242 = DIRECTION ( 'NONE',  ( -1.000000000000000000, -2.999999999999999839E-15, 0.000000000000000000 ) ) ;
#14243 = CARTESIAN_POINT ( 'NONE',  ( 37.12184278917507640, -3.513682088886100452, 71.43714994484035685 ) ) ;
#14244 = CARTESIAN_POINT ( 'NONE',  ( 37.21915885897815457, -7.413682088886101695, 71.08074471024443142 ) ) ;
#14245 = EDGE_LOOP ( 'NONE', ( #4179, #20414, #12136, #5591, #18676, #493, #11668, #20290 ) ) ;
#14246 = ORIENTED_EDGE ( 'NONE', *, *, #19815, .F. ) ;
#14247 = LINE ( 'NONE', #4587, #6217 ) ;
#14248 = ADVANCED_FACE ( 'NONE', ( #20991 ), #4669, .F. ) ;
#14249 = DIRECTION ( 'NONE',  ( 1.734723475976805122E-16, 3.491481338843134933E-15, 1.000000000000000000 ) ) ;
#14250 = ORIENTED_EDGE ( 'NONE', *, *, #11620, .F. ) ;
#14251 = DIRECTION ( 'NONE',  ( -1.000000000000000000, -1.185941393278724777E-16, -8.240782279085522416E-17 ) ) ;
#14252 = CARTESIAN_POINT ( 'NONE',  ( 37.80618814713138676, -11.70384086642190624, 69.62690120949091011 ) ) ;
#14253 = CARTESIAN_POINT ( 'NONE',  ( 43.81606138205700063, -20.45664737071796324, 43.87694304485803798 ) ) ;
#14254 = DIRECTION ( 'NONE',  ( 0.000000000000000000, 0.4425581086832399702, -0.8967398287344626739 ) ) ;
#14255 = ORIENTED_EDGE ( 'NONE', *, *, #24798, .F. ) ;
#14256 = VERTEX_POINT ( 'NONE', #13264 ) ;
#14257 = ORIENTED_EDGE ( 'NONE', *, *, #14290, .F. ) ;
#14258 = CARTESIAN_POINT ( 'NONE',  ( 42.98956905832363873, 3.335839619496017594, 6.349669990344222192 ) ) ;
#14259 = CARTESIAN_POINT ( 'NONE',  ( 39.38009889167650357, -8.213682088886105959, 72.75271321436733274 ) ) ;
#14260 = CARTESIAN_POINT ( 'NONE',  ( 40.31606138205700773, 37.94123852234599781, 74.30501292736988717 ) ) ;
#14261 = LINE ( 'NONE', #10022, #10819 ) ;
#14262 = FACE_OUTER_BOUND ( 'NONE', #11608, .T. ) ;
#14263 = CARTESIAN_POINT ( 'NONE',  ( 36.06606138205697931, -5.948051402551132405, 9.959574150503843981 ) ) ;
#14264 = CARTESIAN_POINT ( 'NONE',  ( 35.81606138205700063, 37.44123852234599781, 75.30501292736990138 ) ) ;
#14265 = DIRECTION ( 'NONE',  ( 0.000000000000000000, 1.000000000000000000, -2.999999999999999839E-15 ) ) ;
#14266 = CARTESIAN_POINT ( 'NONE',  ( 36.31606138205700063, -20.22127907754186893, 75.50705395623725735 ) ) ;
#14267 = ORIENTED_EDGE ( 'NONE', *, *, #7197, .T. ) ;
#14268 = ORIENTED_EDGE ( 'NONE', *, *, #15712, .F. ) ;
#14269 = LINE ( 'NONE', #20195, #7088 ) ;
#14270 = CARTESIAN_POINT ( 'NONE',  ( 36.07789103942399578, -2.203840866421915123, 72.05058123536544201 ) ) ;
#14271 = ORIENTED_EDGE ( 'NONE', *, *, #19884, .F. ) ;
#14272 = EDGE_CURVE ( 'NONE', #19241, #5247, #9284, .T. ) ;
#14273 = CARTESIAN_POINT ( 'NONE',  ( 43.31606138205697221, -3.118133360756952577, 16.65315793475036443 ) ) ;
#14274 = CARTESIAN_POINT ( 'NONE',  ( 38.93415946300897446, -6.113682088886107202, 73.09843995877331224 ) ) ;
#14275 = DIRECTION ( 'NONE',  ( -0.9848643390529194797, 5.199808678756408333E-16, 0.1733269559585469688 ) ) ;
#14276 = CARTESIAN_POINT ( 'NONE',  ( 38.37017380507020192, -14.01368208888610845, 73.71602215082113219 ) ) ;
#14277 = CARTESIAN_POINT ( 'NONE',  ( 43.27190301404667849, 2.993235644242374871, 6.111605774860289664 ) ) ;
#14278 = DIRECTION ( 'NONE',  ( -0.000000000000000000, -3.469446951953613400E-15, -1.000000000000000000 ) ) ;
#14279 = AXIS2_PLACEMENT_3D ( 'NONE', #21064, #10646, #18496 ) ;
#14280 = CARTESIAN_POINT ( 'NONE',  ( 40.31606138205700773, -10.93995761290683255, 80.99653337025984001 ) ) ;
#14281 = EDGE_CURVE ( 'NONE', #19523, #6874, #3463, .T. ) ;
#14282 = AXIS2_PLACEMENT_3D ( 'NONE', #13683, #7635, #21542 ) ;
#14283 = VECTOR ( 'NONE', #21419, 1000.000000000000000 ) ;
#14284 = CARTESIAN_POINT ( 'NONE',  ( 46.81606138205701484, -18.45164032183481595, 27.38658776684409091 ) ) ;
#14285 = ADVANCED_FACE ( 'NONE', ( #19180 ), #15051, .T. ) ;
#14286 = DIRECTION ( 'NONE',  ( -0.000000000000000000, -0.7540134720837717852, -0.6568589528324747517 ) ) ;
#14287 = EDGE_CURVE ( 'NONE', #20891, #13664, #19299, .T. ) ;
#14288 = LINE ( 'NONE', #16086, #15186 ) ;
#14289 = CARTESIAN_POINT ( 'NONE',  ( 38.00113996487114321, -23.91368208888610170, 72.53360434286901182 ) ) ;
#14290 = EDGE_CURVE ( 'NONE', #1954, #8849, #14579, .T. ) ;
#14291 = ORIENTED_EDGE ( 'NONE', *, *, #14301, .T. ) ;
#14292 = FACE_OUTER_BOUND ( 'NONE', #23367, .T. ) ;
#14293 = CARTESIAN_POINT ( 'NONE',  ( 3.816061382056966433, -4.589472609077318133, -6.350807634294847404 ) ) ;
#14294 = ORIENTED_EDGE ( 'NONE', *, *, #21384, .T. ) ;
#14295 = ORIENTED_EDGE ( 'NONE', *, *, #10334, .F. ) ;
#14296 = CARTESIAN_POINT ( 'NONE',  ( 40.55423172469004101, -25.20384086642191690, 70.70992431699446001 ) ) ;
#14297 = EDGE_CURVE ( 'NONE', #23482, #22567, #15701, .T. ) ;
#14298 = CARTESIAN_POINT ( 'NONE',  ( 39.12911128074873801, 1.886317911113891244, 73.69843995877330656 ) ) ;
#14299 = CARTESIAN_POINT ( 'NONE',  ( 45.81606138205706458, -35.90387122078352178, 69.64117576433150703 ) ) ;
#14300 = AXIS2_PLACEMENT_3D ( 'NONE', #16507, #15089, #12920 ) ;
#14301 = EDGE_CURVE ( 'NONE', #25070, #2724, #3331, .T. ) ;
#14302 = CIRCLE ( 'NONE', #12659, 0.9999999999999937828 ) ;
#14303 = AXIS2_PLACEMENT_3D ( 'NONE', #2671, #12864, #24687 ) ;
#14304 = CARTESIAN_POINT ( 'NONE',  ( 32.81606138205700773, -27.17722769842920272, 59.42551550655435477 ) ) ;
#14305 = EDGE_LOOP ( 'NONE', ( #18791, #15770, #8316, #19535 ) ) ;
#14306 = CARTESIAN_POINT ( 'NONE',  ( 44.31606138205700063, -20.55619265724211076, 44.11584019928223910 ) ) ;
#14307 = LINE ( 'NONE', #12257, #950 ) ;
#14308 = CARTESIAN_POINT ( 'NONE',  ( 39.73277004305197124, -5.403840866421909972, 69.52238214136768590 ) ) ;
#14309 = CARTESIAN_POINT ( 'NONE',  ( 42.06606138205700063, 43.19123852234599781, 75.30501292736987295 ) ) ;
#14310 = CARTESIAN_POINT ( 'NONE',  ( 43.31606138205700063, -34.55876147765707174, 70.30501292736873609 ) ) ;
#14311 = CARTESIAN_POINT ( 'NONE',  ( 39.29254315202756231, -8.813682088886100274, 69.94417936956673998 ) ) ;
#14312 = CARTESIAN_POINT ( 'NONE',  ( 34.81606138205700773, -2.300394311618905174, 46.75701924734788406 ) ) ;
#14313 = EDGE_CURVE ( 'NONE', #3261, #1701, #23516, .T. ) ;
#14314 = CARTESIAN_POINT ( 'NONE',  ( 39.29254315202756231, -26.81368208888610027, 69.94417936956671156 ) ) ;
#14315 = CYLINDRICAL_SURFACE ( 'NONE', #17177, 1.000000000000000888 ) ;
#14316 = VECTOR ( 'NONE', #6529, 1000.000000000000000 ) ;
#14317 = CARTESIAN_POINT ( 'NONE',  ( 46.91606138205695231, 0.8576245772853769989, -1.570935883000508460 ) ) ;
#14318 = CARTESIAN_POINT ( 'NONE',  ( 38.37017380507018771, -23.60384086642191903, 70.24448340153875847 ) ) ;
#14319 = CARTESIAN_POINT ( 'NONE',  ( 39.75915168707250302, -14.71368208888610063, 70.26145752964251301 ) ) ;
#14320 = VECTOR ( 'NONE', #3241, 1000.000000000000000 ) ;
#14321 = VECTOR ( 'NONE', #8086, 1000.000000000000000 ) ;
#14322 = ORIENTED_EDGE ( 'NONE', *, *, #12356, .T. ) ;
#14323 = DIRECTION ( 'NONE',  ( 0.000000000000000000, 1.000000000000000000, -2.999999999999998655E-15 ) ) ;
#14324 = CARTESIAN_POINT ( 'NONE',  ( 39.75915168707251723, -10.90384086642191619, 72.49904802271740323 ) ) ;
#14325 = PLANE ( 'NONE',  #6050 ) ;
#14326 = CARTESIAN_POINT ( 'NONE',  ( 39.38009889167650357, -8.213682088886105959, 72.75271321436733274 ) ) ;
#14327 = ORIENTED_EDGE ( 'NONE', *, *, #23246, .T. ) ;
#14328 = CARTESIAN_POINT ( 'NONE',  ( 38.37017380507020192, -16.01368208888610667, 73.71602215082113219 ) ) ;
#14329 = EDGE_LOOP ( 'NONE', ( #21751, #5492, #12852, #20685 ) ) ;
#14330 = CARTESIAN_POINT ( 'NONE',  ( 40.31606138205700773, 5.691238522346996120, 69.09790614618344762 ) ) ;
#14331 = CARTESIAN_POINT ( 'NONE',  ( 30.81606138205696155, 1.773964314019527588, -3.427682652428149623 ) ) ;
#14332 = CARTESIAN_POINT ( 'NONE',  ( 37.38336156205273397, -15.90384086642191264, 70.63227792289247020 ) ) ;
#14333 = ORIENTED_EDGE ( 'NONE', *, *, #15397, .T. ) ;
#14334 = ORIENTED_EDGE ( 'NONE', *, *, #12929, .T. ) ;
#14335 = CARTESIAN_POINT ( 'NONE',  ( 30.81606138205700418, 36.92314894770293421, 79.37823623207323465 ) ) ;
#14336 = DIRECTION ( 'NONE',  ( -2.412663730047099099E-15, 0.8967398287344627850, 0.4425581086832399147 ) ) ;
#14337 = CARTESIAN_POINT ( 'NONE',  ( 39.02088643472237806, -24.70384086642192401, 73.73360434286898624 ) ) ;
#14338 = CARTESIAN_POINT ( 'NONE',  ( 32.84131651066541480, -32.95845724189726411, 59.23979596822106686 ) ) ;
#14339 = CARTESIAN_POINT ( 'NONE',  ( 39.38009889167650357, -28.21368208888610951, 72.75271321436730432 ) ) ;
#14340 = ADVANCED_FACE ( 'NONE', ( #3579 ), #1636, .F. ) ;
#14341 = CARTESIAN_POINT ( 'NONE',  ( 33.31606138205700773, -29.06829118875199924, 75.30501292737000085 ) ) ;
#14342 = ADVANCED_FACE ( 'NONE', ( #25335 ), #17767, .F. ) ;
#14343 = MECHANICAL_DESIGN_GEOMETRIC_PRESENTATION_REPRESENTATION (  '', ( #9829 ), #5698 ) ;
#14344 = VECTOR ( 'NONE', #15322, 1000.000000000000000 ) ;
#14345 = VERTEX_POINT ( 'NONE', #15437 ) ;
#14346 = LINE ( 'NONE', #22199, #19070 ) ;
#14347 = CARTESIAN_POINT ( 'NONE',  ( 33.31606138205700773, -1.357181138186124736, 83.30501292736991559 ) ) ;
#14348 = CARTESIAN_POINT ( 'NONE',  ( 38.93415946300897446, -13.50384086642190518, 69.66206559358663242 ) ) ;
#14349 = SHAPE_REPRESENTATION_RELATIONSHIP ( 'NONE' , 'NONE' ,  #11141, #20268 ) ;
#14350 = CARTESIAN_POINT ( 'NONE',  ( 45.81606138205700063, 46.72314894770294558, 81.17823623207318917 ) ) ;
#14351 = MECHANICAL_DESIGN_GEOMETRIC_PRESENTATION_REPRESENTATION (  '', ( #8604 ), #23386 ) ;
#14352 = EDGE_LOOP ( 'NONE', ( #19142, #19796, #10653, #9438 ) ) ;
#14353 = CARTESIAN_POINT ( 'NONE',  ( 43.81606138205700063, 2.191238522347000117, 69.30501292737000085 ) ) ;
#14354 = DIRECTION ( 'NONE',  ( -1.000000000000000000, 0.000000000000000000, 0.000000000000000000 ) ) ;
#14355 = CARTESIAN_POINT ( 'NONE',  ( 37.89291511884479036, -0.5038408664219118371, 72.49843995877331793 ) ) ;
#14356 = CARTESIAN_POINT ( 'NONE',  ( 43.22322292330370175, 3.253818082689177160, 6.243461734314118772 ) ) ;
#14357 = EDGE_LOOP ( 'NONE', ( #13210, #9344, #22144, #6297 ) ) ;
#14358 = AXIS2_PLACEMENT_3D ( 'NONE', #5580, #9582, #13565 ) ;
#14359 = CARTESIAN_POINT ( 'NONE',  ( 36.06606138205696510, -1.965028424401974227, 1.888915691893686244 ) ) ;
#14360 = ORIENTED_EDGE ( 'NONE', *, *, #8885, .T. ) ;
#14361 = ORIENTED_EDGE ( 'NONE', *, *, #22532, .T. ) ;
#14362 = FACE_OUTER_BOUND ( 'NONE', #15995, .T. ) ;
#14363 = CARTESIAN_POINT ( 'NONE',  ( 39.37952058850012804, -8.613682088886100985, 70.97781676520601479 ) ) ;
#14364 = AXIS2_PLACEMENT_3D ( 'NONE', #10168, #8111, #17913 ) ;
#14365 = CARTESIAN_POINT ( 'NONE',  ( 37.69225076346193504, -1.813682088886100274, 72.33091598616827866 ) ) ;
#14366 = VERTEX_POINT ( 'NONE', #23796 ) ;
#14367 = ORIENTED_EDGE ( 'NONE', *, *, #6273, .F. ) ;
#14368 = DIRECTION ( 'NONE',  ( 1.000000000000000275E-15, -0.9439899321577401858, -0.3299742535180970604 ) ) ;
#14369 = DIRECTION ( 'NONE',  ( 0.000000000000000000, 2.775557561562888984E-15, 1.000000000000000000 ) ) ;
#14370 = DIRECTION ( 'NONE',  ( -1.734723475976814737E-16, 0.000000000000000000, -1.000000000000000000 ) ) ;
#14371 = CARTESIAN_POINT ( 'NONE',  ( 38.37017380507018771, -13.60384086642190837, 69.64448340153877837 ) ) ;
#14372 = EDGE_CURVE ( 'NONE', #7712, #1793, #17638, .T. ) ;
#14373 = VECTOR ( 'NONE', #10687, 1000.000000000000000 ) ;
#14374 = EDGE_CURVE ( 'NONE', #13145, #13325, #6164, .T. ) ;
#14375 = DIRECTION ( 'NONE',  ( 0.000000000000000000, 1.000000000000000000, -2.999999999999999839E-15 ) ) ;
#14376 = EDGE_LOOP ( 'NONE', ( #20027, #9941, #9306, #2773 ) ) ;
#14377 = ORIENTED_EDGE ( 'NONE', *, *, #24955, .T. ) ;
#14378 = ORIENTED_EDGE ( 'NONE', *, *, #6714, .T. ) ;
#14379 = VECTOR ( 'NONE', #19993, 1000.000000000000000 ) ;
#14380 = CARTESIAN_POINT ( 'NONE',  ( 45.81606138205694378, 5.290470704224633280, -0.3848988112044732235 ) ) ;
#14381 = CARTESIAN_POINT ( 'NONE',  ( 40.14115730948191185, -10.51368208888610134, 71.32335560751961623 ) ) ;
#14382 = CARTESIAN_POINT ( 'NONE',  ( 32.81606138205700773, 2.191238522347000117, 69.30501292737000085 ) ) ;
#14383 = CARTESIAN_POINT ( 'NONE',  ( 43.81608638205700146, 0.9984178969752143251, 11.59873562314662010 ) ) ;
#14384 = VECTOR ( 'NONE', #6251, 1000.000000000000000 ) ;
#14385 = DIRECTION ( 'NONE',  ( 0.000000000000000000, 3.469446951953613400E-15, 1.000000000000000000 ) ) ;
#14386 = EDGE_CURVE ( 'NONE', #9404, #23789, #7717, .T. ) ;
#14387 = AXIS2_PLACEMENT_3D ( 'NONE', #5391, #19168, #7836 ) ;
#14388 = LINE ( 'NONE', #10149, #25043 ) ;
#14389 = FACE_OUTER_BOUND ( 'NONE', #18951, .T. ) ;
#14390 = DIRECTION ( 'NONE',  ( 0.000000000000000000, 3.469446951953613400E-15, 1.000000000000000000 ) ) ;
#14391 = ORIENTED_EDGE ( 'NONE', *, *, #11635, .F. ) ;
#14392 = ORIENTED_EDGE ( 'NONE', *, *, #9737, .F. ) ;
#14393 = PRODUCT_DEFINITION_CONTEXT ( 'detailed design', #1713, 'design' ) ;
#14394 = CARTESIAN_POINT ( 'NONE',  ( 37.61123632939164452, 0.2961591335780902612, 69.02690120949095842 ) ) ;
#14395 = AXIS2_PLACEMENT_3D ( 'NONE', #2804, #16217, #24068 ) ;
#14396 = CARTESIAN_POINT ( 'NONE',  ( 38.63098279924288647, -20.91368208888609814, 70.22690120949090442 ) ) ;
#14397 = ORIENTED_EDGE ( 'NONE', *, *, #4913, .T. ) ;
#14398 = EDGE_LOOP ( 'NONE', ( #7282, #940, #12818, #25421, #9173, #18965 ) ) ;
#14399 = DIRECTION ( 'NONE',  ( -2.122643018205887308E-17, 1.000000000000000000, -3.120611096041553009E-15 ) ) ;
#14400 = CARTESIAN_POINT ( 'NONE',  ( 36.68196826583682935, -9.613682088886104538, 71.96809898377890136 ) ) ;
#14401 = CARTESIAN_POINT ( 'NONE',  ( 37.69796330110505522, -28.50384086642191406, 73.09843995877328382 ) ) ;
#14402 = AXIS2_PLACEMENT_3D ( 'NONE', #5241, #20961, #7301 ) ;
#14403 = VECTOR ( 'NONE', #20253, 1000.000000000000227 ) ;
#14404 = CARTESIAN_POINT ( 'NONE',  ( 43.81606138205700063, 35.38401127291550097, 61.48364296169660292 ) ) ;
#14405 = CARTESIAN_POINT ( 'NONE',  ( 36.29569395875879678, -11.31368208888609850, 69.98269868914867686 ) ) ;
#14406 = CIRCLE ( 'NONE', #16870, 4.000000000000000000 ) ;
#14407 = CARTESIAN_POINT ( 'NONE',  ( 40.06606138205700063, 5.308699250829721272, 2.416607620847027960 ) ) ;
#14408 = DIRECTION ( 'NONE',  ( 1.000000000000000000, 0.000000000000000000, 0.000000000000000000 ) ) ;
#14409 = AXIS2_PLACEMENT_3D ( 'NONE', #760, #4397, #22416 ) ;
#14410 = FACE_OUTER_BOUND ( 'NONE', #11649, .T. ) ;
#14411 = PLANE ( 'NONE',  #6673 ) ;
#14412 = APPLICATION_CONTEXT ( 'automotive_design' ) ;
#14413 = CARTESIAN_POINT ( 'NONE',  ( 43.40041788046962523, 3.105313829025544425, 6.135194785527184891 ) ) ;
#14414 = ADVANCED_FACE ( 'NONE', ( #7980 ), #11723, .F. ) ;
#14415 = DIRECTION ( 'NONE',  ( 1.000000000000000000, 0.000000000000000000, 0.000000000000000000 ) ) ;
#14416 = VERTEX_POINT ( 'NONE', #3705 ) ;
#14417 = AXIS2_PLACEMENT_3D ( 'NONE', #19457, #1799, #7879 ) ;
#14418 = DIRECTION ( 'NONE',  ( 1.000000000000000000, 1.000000000000000078E-15, 0.000000000000000000 ) ) ;
#14419 = CARTESIAN_POINT ( 'NONE',  ( 40.31606138205701484, -20.02093502212014897, 26.61211107664843212 ) ) ;
#14420 = VERTEX_POINT ( 'NONE', #23413 ) ;
#14421 = ORIENTED_EDGE ( 'NONE', *, *, #7716, .T. ) ;
#14422 = AXIS2_PLACEMENT_3D ( 'NONE', #13634, #11456, #21489 ) ;
#14423 = CARTESIAN_POINT ( 'NONE',  ( 37.50301148336529877, -24.50384086642192116, 73.69843995877326392 ) ) ;
#14424 = CARTESIAN_POINT ( 'NONE',  ( 39.75915168707250302, -26.71368208888609530, 70.26145752964249880 ) ) ;
#14425 = LINE ( 'NONE', #4390, #405 ) ;
#14426 = EDGE_CURVE ( 'NONE', #18741, #6360, #5780, .T. ) ;
#14427 = CARTESIAN_POINT ( 'NONE',  ( 40.71606138205694947, 3.586515973360791421, -0.5067327973472466329 ) ) ;
#14428 =( NAMED_UNIT ( * ) PLANE_ANGLE_UNIT ( ) SI_UNIT ( $, .RADIAN. ) );
#14429 = ORIENTED_EDGE ( 'NONE', *, *, #5213, .T. ) ;
#14430 = CARTESIAN_POINT ( 'NONE',  ( 31.81606138205700418, 40.39281886181299797, 66.30501292737000085 ) ) ;
#14431 = DIRECTION ( 'NONE',  ( 0.000000000000000000, 0.5706330172266920187, -0.8212051873014210024 ) ) ;
#14432 = CARTESIAN_POINT ( 'NONE',  ( 40.26954217208371034, -24.71368208888610241, 69.89063713639254161 ) ) ;
#14433 = EDGE_CURVE ( 'NONE', #17509, #12956, #19559, .T. ) ;
#14434 = EDGE_CURVE ( 'NONE', #11095, #18567, #19422, .T. ) ;
#14435 = DIRECTION ( 'NONE',  ( 9.027796614315171564E-31, 1.000000000000000000, 1.163336342344335610E-15 ) ) ;
#14436 = CARTESIAN_POINT ( 'NONE',  ( 33.23698021073552411, 3.107177411735388084, 6.136004175196663191 ) ) ;
#14437 = CARTESIAN_POINT ( 'NONE',  ( 38.26194895904383486, -7.013682088886100452, 69.64448340153879258 ) ) ;
#14438 = CARTESIAN_POINT ( 'NONE',  ( 33.31606138205700773, -19.34822312381090370, 24.15308711316412627 ) ) ;
#14439 = AXIS2_PLACEMENT_3D ( 'NONE', #10567, #752, #8638 ) ;
#14440 = CARTESIAN_POINT ( 'NONE',  ( 39.98359781491296161, -18.41368208888610880, 71.86517103874047052 ) ) ;
#14441 = CIRCLE ( 'NONE', #12397, 0.7499999999999997780 ) ;
#14442 = CARTESIAN_POINT ( 'NONE',  ( 40.31606138205700773, 42.19123852234596939, 65.30501292736988717 ) ) ;
#14443 = EDGE_CURVE ( 'NONE', #4268, #9258, #4235, .T. ) ;
#14444 = DIRECTION ( 'NONE',  ( 0.000000000000000000, -1.000000000000000000, 3.325260651745651169E-15 ) ) ;
#14445 = CARTESIAN_POINT ( 'NONE',  ( 39.02742774030101458, -25.40384086642191264, 70.49320253461758057 ) ) ;
#14446 = CARTESIAN_POINT ( 'NONE',  ( 37.33957961208646736, -11.81368208888610916, 72.81632618279321889 ) ) ;
#14447 = DIRECTION ( 'NONE',  ( 0.000000000000000000, -0.7516416929448823669, -0.6595716529892345914 ) ) ;
#14448 = ORIENTED_EDGE ( 'NONE', *, *, #11460, .T. ) ;
#14449 = CARTESIAN_POINT ( 'NONE',  ( 40.14115730948191185, -11.10384086642191015, 71.43714994484034264 ) ) ;
#14450 = DIRECTION ( 'NONE',  ( -1.225631768639319301E-15, 0.4425581086832399147, -0.8967398287344627850 ) ) ;
#14451 = CARTESIAN_POINT ( 'NONE',  ( 38.37017380507020192, -8.013682088886108446, 73.11602215082118050 ) ) ;
#14452 = ORIENTED_EDGE ( 'NONE', *, *, #10053, .F. ) ;
#14453 = CARTESIAN_POINT ( 'NONE',  ( 36.98690846071097837, -17.81368208888610738, 73.30173637941818754 ) ) ;
#14454 = ORIENTED_EDGE ( 'NONE', *, *, #1528, .F. ) ;
#14455 = CARTESIAN_POINT ( 'NONE',  ( 33.40064408022072939, 41.67000142393845152, 79.87823623207322044 ) ) ;
#14456 = CARTESIAN_POINT ( 'NONE',  ( 42.82259739205072435, 3.224889171211050343, 6.370942055173422602 ) ) ;
#14457 = CIRCLE ( 'NONE', #9529, 1.750000000000001998 ) ;
#14458 = CARTESIAN_POINT ( 'NONE',  ( 38.26194895904384197, -10.60384086642191370, 72.51602215082118619 ) ) ;
#14459 = ORIENTED_EDGE ( 'NONE', *, *, #6042, .F. ) ;
#14460 = ORIENTED_EDGE ( 'NONE', *, *, #14600, .T. ) ;
#14461 = DIRECTION ( 'NONE',  ( -1.000000000000000000, -2.999999999999999839E-15, 0.000000000000000000 ) ) ;
#14462 = CARTESIAN_POINT ( 'NONE',  ( 0.000000000000000000, 46.72314894770294558, 81.37823623207320622 ) ) ;
#14463 = CARTESIAN_POINT ( 'NONE',  ( 40.77203464402485622, -21.10384086642191548, 71.43714994484032843 ) ) ;
#14464 = EDGE_CURVE ( 'NONE', #9599, #17216, #14024, .T. ) ;
#14465 = EDGE_CURVE ( 'NONE', #21608, #13262, #21880, .T. ) ;
#14466 = DIRECTION ( 'NONE',  ( 0.000000000000000000, 2.999999999999999839E-15, 1.000000000000000000 ) ) ;
#14467 = CARTESIAN_POINT ( 'NONE',  ( 39.38009889167650357, -24.21368208888610596, 72.75271321436730432 ) ) ;
#14468 = CARTESIAN_POINT ( 'NONE',  ( 36.31606138205700063, 39.69123852234599070, 73.55501292736988717 ) ) ;
#14469 = CARTESIAN_POINT ( 'NONE',  ( 44.31606138205700063, 10.06218483883314718, 67.80501292737497465 ) ) ;
#14470 = VERTEX_POINT ( 'NONE', #2030 ) ;
#14471 = CARTESIAN_POINT ( 'NONE',  ( 30.81606138205700418, -11.72563467517899838, 72.98595903681224684 ) ) ;
#14472 = CARTESIAN_POINT ( 'NONE',  ( 43.31606138205700063, -13.25716901376041967, 21.21736665487721041 ) ) ;
#14473 = EDGE_CURVE ( 'NONE', #20798, #17007, #9960, .T. ) ;
#14474 = CARTESIAN_POINT ( 'NONE',  ( 39.38009889167648936, -13.40384086642191086, 70.00779233799262613 ) ) ;
#14475 = VECTOR ( 'NONE', #13951, 1000.000000000000000 ) ;
#14476 = CARTESIAN_POINT ( 'NONE',  ( 32.81606138205700773, 46.72314894770294558, 81.17823623207320338 ) ) ;
#14477 = VERTEX_POINT ( 'NONE', #13893 ) ;
#14478 = LINE ( 'NONE', #18473, #4088 ) ;
#14479 = LINE ( 'NONE', #24120, #21815 ) ;
#14480 = CARTESIAN_POINT ( 'NONE',  ( 36.80608444377001831, -28.30384086642191122, 72.40698646996133903 ) ) ;
#14481 = LINE ( 'NONE', #18353, #17998 ) ;
#14482 = ORIENTED_EDGE ( 'NONE', *, *, #18072, .T. ) ;
#14483 = EDGE_CURVE ( 'NONE', #23154, #16840, #1768, .T. ) ;
#14484 = CARTESIAN_POINT ( 'NONE',  ( 36.80608444377001121, -27.31368208888610383, 70.35351908239857721 ) ) ;
#14485 = ORIENTED_EDGE ( 'NONE', *, *, #2320, .F. ) ;
#14486 = ORIENTED_EDGE ( 'NONE', *, *, #7973, .T. ) ;
#14487 = CYLINDRICAL_SURFACE ( 'NONE', #5340, 2.000000000000001776 ) ;
#14488 = CARTESIAN_POINT ( 'NONE',  ( 33.31606138205700773, 2.476587234117772596, 12.62587505415466538 ) ) ;
#14489 = CARTESIAN_POINT ( 'NONE',  ( 39.24876120206128860, -2.713682088886101962, 70.63227792289247020 ) ) ;
#14490 = CARTESIAN_POINT ( 'NONE',  ( 39.37952058850012804, -0.6136820888861006518, 70.97781676520601479 ) ) ;
#14491 = ORIENTED_EDGE ( 'NONE', *, *, #9232, .F. ) ;
#14492 = EDGE_LOOP ( 'NONE', ( #14897, #14023, #18744, #4192 ) ) ;
#14493 = LINE ( 'NONE', #20299, #25108 ) ;
#14494 = CARTESIAN_POINT ( 'NONE',  ( 40.31606138205701484, -23.16691978223481385, 31.29201591705069063 ) ) ;
#14495 = ORIENTED_EDGE ( 'NONE', *, *, #7373, .F. ) ;
#14496 = CIRCLE ( 'NONE', #20243, 3.000000000000000444 ) ;
#14497 = CARTESIAN_POINT ( 'NONE',  ( 36.64852494920107517, -8.203840866421909794, 71.86517103874049894 ) ) ;
#14498 = VECTOR ( 'NONE', #23145, 1000.000000000000000 ) ;
#14499 = DIRECTION ( 'NONE',  ( -1.225631768639319301E-15, 0.4425581086832399147, -0.8967398287344627850 ) ) ;
#14500 = CIRCLE ( 'NONE', #11235, 2.999999999999998668 ) ;
#14501 = FACE_OUTER_BOUND ( 'NONE', #23405, .T. ) ;
#14502 = ORIENTED_EDGE ( 'NONE', *, *, #3158, .T. ) ;
#14503 = ORIENTED_EDGE ( 'NONE', *, *, #7743, .F. ) ;
#14504 = ORIENTED_EDGE ( 'NONE', *, *, #94, .F. ) ;
#14505 = CARTESIAN_POINT ( 'NONE',  ( 43.81606138205700063, 35.38401127291550097, 61.48364296169660292 ) ) ;
#14506 = CARTESIAN_POINT ( 'NONE',  ( 39.29254315202756231, -4.813682088886099386, 69.94417936956673998 ) ) ;
#14507 = VECTOR ( 'NONE', #2670, 1000.000000000000000 ) ;
#14508 = DIRECTION ( 'NONE',  ( 0.000000000000000000, 2.999999999999999839E-15, 1.000000000000000000 ) ) ;
#14509 = CARTESIAN_POINT ( 'NONE',  ( 32.81606138205700773, -35.70002751211045933, 71.94742330197156832 ) ) ;
#14510 = DIRECTION ( 'NONE',  ( -1.123589211228918605E-15, 0.4425581086832399147, -0.8967398287344627850 ) ) ;
#14511 = VECTOR ( 'NONE', #22870, 1000.000000000000000 ) ;
#14512 = ADVANCED_FACE ( 'NONE', ( #2158 ), #10035, .F. ) ;
#14513 = LINE ( 'NONE', #7172, #21369 ) ;
#14514 = CARTESIAN_POINT ( 'NONE',  ( 36.31606138205701484, -18.91453975041206093, 24.37026150481227305 ) ) ;
#14515 = ADVANCED_FACE ( 'NONE', ( #8099 ), #15942, .F. ) ;
#14516 = AXIS2_PLACEMENT_3D ( 'NONE', #19275, #25313, #17735 ) ;
#14517 = DIRECTION ( 'NONE',  ( 0.000000000000000000, 0.000000000000000000, -1.000000000000000000 ) ) ;
#14518 = ORIENTED_EDGE ( 'NONE', *, *, #12906, .F. ) ;
#14519 = ORIENTED_EDGE ( 'NONE', *, *, #22711, .F. ) ;
#14520 = LINE ( 'NONE', #10408, #22289 ) ;
#14521 = CARTESIAN_POINT ( 'NONE',  ( 36.29569395875879678, -27.31368208888610027, 69.98269868914866265 ) ) ;
#14522 = CARTESIAN_POINT ( 'NONE',  ( 38.73920764526925353, -22.11368208888610098, 72.49843995877330372 ) ) ;
#14523 = ORIENTED_EDGE ( 'NONE', *, *, #21529, .F. ) ;
#14524 = AXIS2_PLACEMENT_3D ( 'NONE', #17359, #17111, #7828 ) ;
#14525 = ORIENTED_EDGE ( 'NONE', *, *, #25160, .F. ) ;
#14526 = CARTESIAN_POINT ( 'NONE',  ( 32.31606138205700063, 10.06218483883314718, 67.80501292737497465 ) ) ;
#14527 = CARTESIAN_POINT ( 'NONE',  ( 38.93415946300897446, -2.113682088886109423, 73.09843995877331224 ) ) ;
#14528 = CARTESIAN_POINT ( 'NONE',  ( 38.63098279924290068, 1.296159133578087763, 72.53360434286905445 ) ) ;
#14529 = DIRECTION ( 'NONE',  ( 1.000000000000000000, 0.000000000000000000, 0.000000000000000000 ) ) ;
#14530 = EDGE_CURVE ( 'NONE', #9369, #16916, #11197, .T. ) ;
#14531 = AXIS2_PLACEMENT_3D ( 'NONE', #8285, #12414, #22055 ) ;
#14532 = CARTESIAN_POINT ( 'NONE',  ( 39.64521430340304420, -8.813682088886096722, 69.45876917294177133 ) ) ;
#14533 = AXIS2_PLACEMENT_3D ( 'NONE', #673, #6866, #18470 ) ;
#14534 = CYLINDRICAL_SURFACE ( 'NONE', #4914, 3.000000000000002665 ) ;
#14535 = CYLINDRICAL_SURFACE ( 'NONE', #8356, 1.250000000000001110 ) ;
#14536 = AXIS2_PLACEMENT_3D ( 'NONE', #33, #7913, #21432 ) ;
#14537 = CARTESIAN_POINT ( 'NONE',  ( 47.84183937708599643, -33.05991196579839198, 70.24627502810386659 ) ) ;
#14538 = CARTESIAN_POINT ( 'NONE',  ( 43.29451156103230858, 3.885829148717482973, 6.335591667789099546 ) ) ;
#14539 = CARTESIAN_POINT ( 'NONE',  ( 43.52775316163927499, 3.233996417830672154, 6.148606455994836573 ) ) ;
#14540 = LINE ( 'NONE', #6813, #10259 ) ;
#14541 = ORIENTED_EDGE ( 'NONE', *, *, #24306, .T. ) ;
#14542 = CARTESIAN_POINT ( 'NONE',  ( 38.31606138205700063, -22.22127907754186893, 75.30501292736998664 ) ) ;
#14543 = DIRECTION ( 'NONE',  ( 1.000000000000000000, 3.388898908187273079E-15, 1.919289851541777660E-16 ) ) ;
#14544 = VERTEX_POINT ( 'NONE', #17512 ) ;
#14545 = ORIENTED_EDGE ( 'NONE', *, *, #19966, .F. ) ;
#14546 = CARTESIAN_POINT ( 'NONE',  ( 39.64521430340305841, -18.80384086642191477, 73.30173637941818754 ) ) ;
#14547 = AXIS2_PLACEMENT_3D ( 'NONE', #17672, #9696, #23582 ) ;
#14548 = CARTESIAN_POINT ( 'NONE',  ( 38.93415946300897446, -22.11368208888610454, 73.09843995877329803 ) ) ;
#14549 = DIRECTION ( 'NONE',  ( -0.000000000000000000, -3.469446951953613400E-15, -1.000000000000000000 ) ) ;
#14550 = CARTESIAN_POINT ( 'NONE',  ( 32.81606138205700773, -35.82531359714782582, 71.25150419970752580 ) ) ;
#14551 = SURFACE_STYLE_FILL_AREA ( #16231 ) ;
#14552 = ORIENTED_EDGE ( 'NONE', *, *, #1302, .F. ) ;
#14553 = CARTESIAN_POINT ( 'NONE',  ( 33.81606138205700063, 15.19123852234700323, 70.30501292736995822 ) ) ;
#14554 = CYLINDRICAL_SURFACE ( 'NONE', #13335, 1.000000000000000888 ) ;
#14555 = EDGE_CURVE ( 'NONE', #7685, #18110, #2534, .T. ) ;
#14556 = CARTESIAN_POINT ( 'NONE',  ( 37.50301148336529167, -27.11368208888610454, 69.06206559358663810 ) ) ;
#14557 = ORIENTED_EDGE ( 'NONE', *, *, #5900, .F. ) ;
#14558 = DIRECTION ( 'NONE',  ( -1.000000000000000000, -0.000000000000000000, 0.000000000000000000 ) ) ;
#14559 = CARTESIAN_POINT ( 'NONE',  ( 43.31606138205700063, -5.204193249396277032, 83.30501292736992980 ) ) ;
#14560 = CARTESIAN_POINT ( 'NONE',  ( 39.82603832034400426, 1.686317911113891732, 72.40698646996136745 ) ) ;
#14561 = CARTESIAN_POINT ( 'NONE',  ( 36.31606138205700063, -10.19550266980813369, 14.63954348514304904 ) ) ;
#14562 = CARTESIAN_POINT ( 'NONE',  ( 40.14115730948191185, -18.51368208888610312, 71.32335560751960202 ) ) ;
#14563 = CARTESIAN_POINT ( 'NONE',  ( 41.31606138205700063, 2.715274261285174351, 65.05190033008260286 ) ) ;
#14564 = CIRCLE ( 'NONE', #6338, 0.7500000000000006661 ) ;
#14565 = CARTESIAN_POINT ( 'NONE',  ( 34.56606138205700773, 43.19123852234599781, 74.30501292736987295 ) ) ;
#14566 = CARTESIAN_POINT ( 'NONE',  ( 38.26194895904384197, -24.60384086642190837, 72.51602215082114355 ) ) ;
#14567 = CARTESIAN_POINT ( 'NONE',  ( 38.82593461698262871, -8.913682088886101695, 69.62690120949091011 ) ) ;
#14568 = ORIENTED_EDGE ( 'NONE', *, *, #13379, .T. ) ;
#14569 = CARTESIAN_POINT ( 'NONE',  ( 41.96606138205694236, 6.105630034208208379, 5.871938670042847974 ) ) ;
#14570 = VERTEX_POINT ( 'NONE', #473 ) ;
#14571 = CARTESIAN_POINT ( 'NONE',  ( 36.80608444377001831, -4.303840866421916544, 72.40698646996136745 ) ) ;
#14572 = DIRECTION ( 'NONE',  ( 1.000000000000000000, 0.000000000000000000, 0.000000000000000000 ) ) ;
#14573 = AXIS2_PLACEMENT_3D ( 'NONE', #16661, #4568, #12566 ) ;
#14574 = CARTESIAN_POINT ( 'NONE',  ( 39.38009889167650357, -6.213682088886108623, 72.75271321436733274 ) ) ;
#14575 = ORIENTED_EDGE ( 'NONE', *, *, #16496, .T. ) ;
#14576 = CARTESIAN_POINT ( 'NONE',  ( 40.52078840805428683, -14.61368208888610276, 70.60699637195608602 ) ) ;
#14577 = VERTEX_POINT ( 'NONE', #20331 ) ;
#14578 = CARTESIAN_POINT ( 'NONE',  ( 43.31606138205700063, -12.97731741051367393, 21.08248588348817876 ) ) ;
#14579 = LINE ( 'NONE', #21238, #22707 ) ;
#14580 = CARTESIAN_POINT ( 'NONE',  ( 38.93987200065210175, -10.80384086642191299, 72.33091598616827866 ) ) ;
#14581 = CARTESIAN_POINT ( 'NONE',  ( 35.64099152588522657, 1.142818861812999742, 84.30501292737000085 ) ) ;
#14582 = ORIENTED_EDGE ( 'NONE', *, *, #3445, .F. ) ;
#14583 = CARTESIAN_POINT ( 'NONE',  ( 38.41621794735363693, -38.10729675983899511, 83.30501292737011454 ) ) ;
#14584 = DIRECTION ( 'NONE',  ( -1.000000000000000000, 0.000000000000000000, 0.000000000000000000 ) ) ;
#14585 = ADVANCED_FACE ( 'NONE', ( #16071 ), #725, .F. ) ;
#14586 = CARTESIAN_POINT ( 'NONE',  ( 40.77203464402485622, -17.10384086642191193, 71.43714994484032843 ) ) ;
#14587 = SHAPE_REPRESENTATION ( 'Follower', ( #2000 ), #17034 ) ;
#14588 = DIRECTION ( 'NONE',  ( 0.000000000000000000, -1.000000000000000000, 2.999999999999999839E-15 ) ) ;
#14589 = CARTESIAN_POINT ( 'NONE',  ( 32.56606138205700773, 40.39281886181299797, 83.30501292736984453 ) ) ;
#14590 = CARTESIAN_POINT ( 'NONE',  ( 36.87297107704152666, -25.71368208888609885, 72.49904802271738902 ) ) ;
#14591 = CARTESIAN_POINT ( 'NONE',  ( 40.81606138205700773, 41.44123852234599781, 74.30501292736987295 ) ) ;
#14592 = DIRECTION ( 'NONE',  ( 1.000000000000000000, 0.000000000000000000, -0.000000000000000000 ) ) ;
#14593 = ORIENTED_EDGE ( 'NONE', *, *, #14621, .F. ) ;
#14594 = CARTESIAN_POINT ( 'NONE',  ( 33.31606138205700773, -34.55876147765707174, 70.30501292736873609 ) ) ;
#14595 = CARTESIAN_POINT ( 'NONE',  ( 33.31606138205700773, -11.22674583108233115, 81.40610939240433197 ) ) ;
#14596 = CARTESIAN_POINT ( 'NONE',  ( 36.49096545463212493, -14.10384086642191193, 71.32335560751961623 ) ) ;
#14597 = DIRECTION ( 'NONE',  ( 0.000000000000000000, 0.000000000000000000, 1.000000000000000000 ) ) ;
#14598 = DIRECTION ( 'NONE',  ( 0.000000000000000000, -0.8212051873014203363, -0.5706330172266926848 ) ) ;
#14599 = EDGE_CURVE ( 'NONE', #7272, #11199, #8733, .T. ) ;
#14600 = EDGE_CURVE ( 'NONE', #848, #19678, #10414, .T. ) ;
#14601 = DIRECTION ( 'NONE',  ( -1.327674326049719602E-15, 0.4425581086832399147, -0.8967398287344627850 ) ) ;
#14602 = EDGE_CURVE ( 'NONE', #13002, #2254, #23108, .T. ) ;
#14603 = CARTESIAN_POINT ( 'NONE',  ( 44.06606138205700063, 0.6124887759231013584, 82.37823623207334833 ) ) ;
#14604 = EDGE_CURVE ( 'NONE', #6883, #24859, #14154, .T. ) ;
#14605 = CARTESIAN_POINT ( 'NONE',  ( 39.82603832034400426, -29.30384086642190766, 70.35351908239857721 ) ) ;
#14606 = EDGE_CURVE ( 'NONE', #5217, #4779, #8226, .T. ) ;
#14607 = CARTESIAN_POINT ( 'NONE',  ( 37.66883992158368955, -22.12333347212302925, 75.80539787555638043 ) ) ;
#14608 = EDGE_LOOP ( 'NONE', ( #23067, #25174 ) ) ;
#14609 = CARTESIAN_POINT ( 'NONE',  ( 37.69796330110504101, -23.11368208888609743, 69.66206559358660400 ) ) ;
#14610 = ORIENTED_EDGE ( 'NONE', *, *, #7661, .T. ) ;
#14611 = VERTEX_POINT ( 'NONE', #4860 ) ;
#14612 = CARTESIAN_POINT ( 'NONE',  ( 42.85693730032902238, 2.786099971025956190, 6.091850983466585490 ) ) ;
#14613 = DIRECTION ( 'NONE',  ( 0.000000000000000000, 1.000000000000000000, 0.000000000000000000 ) ) ;
#14614 = CARTESIAN_POINT ( 'NONE',  ( 39.31564783533280405, 1.686317911113899282, 72.03616607671141026 ) ) ;
#14615 = CARTESIAN_POINT ( 'NONE',  ( 39.51027997493896748, -0.5136820888861012291, 71.32335560751961623 ) ) ;
#14616 = ORIENTED_EDGE ( 'NONE', *, *, #14894, .T. ) ;
#14617 = ORIENTED_EDGE ( 'NONE', *, *, #19731, .T. ) ;
#14618 = CARTESIAN_POINT ( 'NONE',  ( 35.31606138205687273, 43.19123852234595518, 61.80501292736988006 ) ) ;
#14619 = CARTESIAN_POINT ( 'NONE',  ( 29.81606138205697221, -3.227578639999851617, -4.500312080287595329 ) ) ;
#14620 = ORIENTED_EDGE ( 'NONE', *, *, #11310, .F. ) ;
#14621 = EDGE_CURVE ( 'NONE', #2625, #15873, #22254, .T. ) ;
#14622 = FACE_OUTER_BOUND ( 'NONE', #11669, .T. ) ;
#14623 = CARTESIAN_POINT ( 'NONE',  ( 37.80618814713138676, -7.703840866421907130, 69.62690120949091011 ) ) ;
#14624 = EDGE_CURVE ( 'NONE', #23772, #9515, #4739, .T. ) ;
#14625 = CARTESIAN_POINT ( 'NONE',  ( 35.31606138205687273, 33.19123852234596939, 65.30501292736991559 ) ) ;
#14626 = CARTESIAN_POINT ( 'NONE',  ( 43.31606138205700063, -14.32738121993773994, 11.12118157620986558 ) ) ;
#14627 = ORIENTED_EDGE ( 'NONE', *, *, #16641, .F. ) ;
#14628 = ORIENTED_EDGE ( 'NONE', *, *, #12289, .F. ) ;
#14629 = ORIENTED_EDGE ( 'NONE', *, *, #25469, .T. ) ;
#14630 = DIRECTION ( 'NONE',  ( 0.000000000000000000, 0.8967398287344625629, 0.4425581086832402478 ) ) ;
#14631 = CARTESIAN_POINT ( 'NONE',  ( 39.82603832034401847, -6.313682088886107380, 72.40698646996133903 ) ) ;
#14632 = EDGE_CURVE ( 'NONE', #20287, #14416, #12026, .T. ) ;
#14633 = CARTESIAN_POINT ( 'NONE',  ( 31.81606138205700418, -34.55876147765410167, 70.30501292737000085 ) ) ;
#14634 = DIRECTION ( 'NONE',  ( 0.000000000000000000, -0.4278636397681519488, 0.9038432971286277651 ) ) ;
#14635 = CARTESIAN_POINT ( 'NONE',  ( 40.71606138205696368, 0.5799492015812739432, -3.145019409304214530 ) ) ;
#14636 = CARTESIAN_POINT ( 'NONE',  ( 35.64099152588522657, -0.6071811381869983704, 80.05501292737000085 ) ) ;
#14637 = LINE ( 'NONE', #12977, #11836 ) ;
#14638 = CARTESIAN_POINT ( 'NONE',  ( 46.81606138205705747, -33.21365173458013231, 70.96885009038120984 ) ) ;
#14639 = ORIENTED_EDGE ( 'NONE', *, *, #22713, .T. ) ;
#14640 = EDGE_LOOP ( 'NONE', ( #5843, #25314, #20428, #3867 ) ) ;
#14641 = DIRECTION ( 'NONE',  ( 0.000000000000000000, 1.000000000000000000, 0.000000000000000000 ) ) ;
#14642 = CARTESIAN_POINT ( 'NONE',  ( 40.26954217208372455, 1.096159133578081812, 72.86986841596736042 ) ) ;
#14643 = LINE ( 'NONE', #18768, #9066 ) ;
#14644 = CARTESIAN_POINT ( 'NONE',  ( 37.69225076346193504, -19.81368208888610383, 72.33091598616826445 ) ) ;
#14645 = VERTEX_POINT ( 'NONE', #2663 ) ;
#14646 = ORIENTED_EDGE ( 'NONE', *, *, #2147, .F. ) ;
#14647 = CARTESIAN_POINT ( 'NONE',  ( 39.81746892067405952, 41.67000142393845152, 79.52109337493035923 ) ) ;
#14648 = CARTESIAN_POINT ( 'NONE',  ( 37.69796330110504101, -5.113682088886101873, 69.66206559358663242 ) ) ;
#14649 = CARTESIAN_POINT ( 'NONE',  ( 39.29254315202757653, -28.80384086642191832, 72.81632618279320468 ) ) ;
#14650 = CARTESIAN_POINT ( 'NONE',  ( 17.31606138205699708, 34.87886987267149408, 81.44836866983821722 ) ) ;
#14651 = CARTESIAN_POINT ( 'NONE',  ( 35.86008812008917346, -5.513682088886105781, 71.43714994484035685 ) ) ;
#14652 = DIRECTION ( 'NONE',  ( -3.469446951953616555E-15, 0.8967398287344632291, 0.4425581086832389155 ) ) ;
#14653 = CARTESIAN_POINT ( 'NONE',  ( 40.81606138205700773, -31.05876147765399864, 74.30501292737010033 ) ) ;
#14654 = DIRECTION ( 'NONE',  ( -1.734723475976804876E-16, -3.430248998885765387E-15, -1.000000000000000000 ) ) ;
#14655 = CARTESIAN_POINT ( 'NONE',  ( 30.81606138205700418, 36.92314894770294131, 80.37823623207322044 ) ) ;
#14656 = CARTESIAN_POINT ( 'NONE',  ( 43.20275628853117666, 3.610264363385236930, 6.334189765992617183 ) ) ;
#14657 = CARTESIAN_POINT ( 'NONE',  ( 36.06606138205700063, 5.308699250829721272, 2.416607620847027960 ) ) ;
#14658 = FACE_OUTER_BOUND ( 'NONE', #5102, .T. ) ;
#14659 = ORIENTED_EDGE ( 'NONE', *, *, #20604, .T. ) ;
#14660 = CARTESIAN_POINT ( 'NONE',  ( 40.31606138205700773, -20.32127907754186680, 75.99695190479390305 ) ) ;
#14661 = DIRECTION ( 'NONE',  ( 0.000000000000000000, 2.999999999999999839E-15, 1.000000000000000000 ) ) ;
#14662 = ORIENTED_EDGE ( 'NONE', *, *, #7234, .T. ) ;
#14663 = ORIENTED_EDGE ( 'NONE', *, *, #9417, .T. ) ;
#14664 = UNCERTAINTY_MEASURE_WITH_UNIT (LENGTH_MEASURE( 1.000000000000000082E-05 ), #11413, 'distance_accuracy_value', 'NONE');
#14665 = CARTESIAN_POINT ( 'NONE',  ( 40.77203464402485622, -17.10384086642191193, 71.43714994484032843 ) ) ;
#14666 = CARTESIAN_POINT ( 'NONE',  ( 36.68196826583682935, -19.61368208888610809, 71.96809898377888715 ) ) ;
#14667 = FACE_OUTER_BOUND ( 'NONE', #16778, .T. ) ;
#14668 = CARTESIAN_POINT ( 'NONE',  ( 41.81606138205696510, -1.975699482566714904, -4.057200616784870206 ) ) ;
#14669 = ORIENTED_EDGE ( 'NONE', *, *, #17940, .T. ) ;
#14670 = DIRECTION ( 'NONE',  ( 0.000000000000000000, 2.999999999999999839E-15, 1.000000000000000000 ) ) ;
#14671 = DIRECTION ( 'NONE',  ( 0.000000000000000000, -0.5706330172266952383, 0.8212051873014186709 ) ) ;
#14672 = CARTESIAN_POINT ( 'NONE',  ( 39.02088643472237806, 1.296159133578080658, 73.73360434286904308 ) ) ;
#14673 = VECTOR ( 'NONE', #24398, 1000.000000000000000 ) ;
#14674 = ORIENTED_EDGE ( 'NONE', *, *, #13973, .F. ) ;
#14675 = ADVANCED_FACE ( 'NONE', ( #12734 ), #12359, .F. ) ;
#14676 = CARTESIAN_POINT ( 'NONE',  ( 39.31606138205702194, -21.37925193044962313, 31.05911325134166034 ) ) ;
#14678 = EDGE_CURVE ( 'NONE', #22327, #1199, #880, .T. ) ;
#14677 = FACE_OUTER_BOUND ( 'NONE', #20553, .T. ) ;
#14679 = AXIS2_PLACEMENT_3D ( 'NONE', #19896, #18345, #22200 ) ;
#14680 = VECTOR ( 'NONE', #6246, 999.9999999999998863 ) ;
#14681 = CARTESIAN_POINT ( 'NONE',  ( 39.75915168707250302, -2.713682088886101962, 70.26145752964252722 ) ) ;
#14682 = DIRECTION ( 'NONE',  ( 0.000000000000000000, -3.491481338843135327E-15, -1.000000000000000000 ) ) ;
#14683 = CARTESIAN_POINT ( 'NONE',  ( 38.26194895904383486, -21.01368208888610312, 69.64448340153877837 ) ) ;
#14684 = SHAPE_REPRESENTATION ( 'Metal Base Plate', ( #2000 ), #15777 ) ;
#14685 = PLANE ( 'NONE',  #2046 ) ;
#14686 = DIRECTION ( 'NONE',  ( 1.849283715844614949E-16, -0.8212051873014210024, -0.5706330172266920187 ) ) ;
#14687 = CARTESIAN_POINT ( 'NONE',  ( 37.38336156205273397, -15.90384086642191264, 70.63227792289247020 ) ) ;
#14688 = CARTESIAN_POINT ( 'NONE',  ( 38.82593461698262871, -4.913682088886100807, 69.62690120949091011 ) ) ;
#14689 = ORIENTED_EDGE ( 'NONE', *, *, #13412, .T. ) ;
#14690 = DIRECTION ( 'NONE',  ( 0.000000000000000000, 1.000000000000000000, 0.000000000000000000 ) ) ;
#14691 = EDGE_CURVE ( 'NONE', #15969, #981, #24050, .T. ) ;
#14692 = EDGE_LOOP ( 'NONE', ( #1045, #654, #6406, #15415, #20632, #11392, #24441, #19030, #16295, #9505, #8389, #9549, #10002, #6271, #6827, #6843 ) ) ;
#14693 = CLOSED_SHELL ( 'NONE', ( #24691, #24352, #20613, #3802, #16174, #7697, #13825, #4618, #6659, #24047, #19715, #4025, #7532, #23233, #8238, #22772, #23024, #13814, #16463, #10835, #5477, #394, #2019, #17660, #14049, #13223, #4689, #16189, #3720, #14515, #3761, #7132, #6120, #10931, #19175, #13510, #12231, #18882, #18585, #18232, #10466, #15527, #11319, #12748, #11162, #2292, #7987, #22247, #6579, #4428, #10518, #9913, #10677, #11758, #10291, #17475, #24493, #19663, #25205, #2330, #12321, #4979, #6458, #10917, #5558, #2020, #14585, #6485, #1675, #15068, #10836, #19869, #8783, #18490, #24268, #9276, #14785, #2605, #19293, #16390, #21848, #12504, #21374, #21866, #6809, #8803, #4463, #10331, #19008, #11952, #22961, #15847, #10453, #7923, #14675, #10366, #14204, #16358 ) ) ;
#14694 = CARTESIAN_POINT ( 'NONE',  ( 38.37017380507018771, -7.603840866421906597, 69.64448340153879258 ) ) ;
#14695 = DIRECTION ( 'NONE',  ( 9.027796614315171564E-31, 1.000000000000000000, 3.938893903907230117E-15 ) ) ;
#14696 = VECTOR ( 'NONE', #13686, 1000.000000000000000 ) ;
#14697 = AXIS2_PLACEMENT_3D ( 'NONE', #3693, #1622, #19410 ) ;
#14698 = CARTESIAN_POINT ( 'NONE',  ( 39.75915168707250302, -2.713682088886101962, 70.26145752964252722 ) ) ;
#14699 = ORIENTED_EDGE ( 'NONE', *, *, #17781, .F. ) ;
#14700 = CARTESIAN_POINT ( 'NONE',  ( 40.77203464402485622, -8.513682088886104893, 71.32335560751961623 ) ) ;
#14701 = ORIENTED_EDGE ( 'NONE', *, *, #10645, .T. ) ;
#14702 = CARTESIAN_POINT ( 'NONE',  ( 33.66606138205693810, 6.105630034208183510, 5.871938670042847974 ) ) ;
#14703 = CARTESIAN_POINT ( 'NONE',  ( 39.02742774030101458, -11.40384086642191086, 70.49320253461759478 ) ) ;
#14704 = ORIENTED_EDGE ( 'NONE', *, *, #4232, .F. ) ;
#14705 = EDGE_LOOP ( 'NONE', ( #2512, #20036, #22751, #24218 ) ) ;
#14706 = LINE ( 'NONE', #14968, #25262 ) ;
#14707 = DIRECTION ( 'NONE',  ( 2.792262043613788535E-15, -0.8967398287344627850, -0.4425581086832399147 ) ) ;
#14708 = CARTESIAN_POINT ( 'NONE',  ( 40.33642880535521869, -15.30384086642191477, 69.98269868914866265 ) ) ;
#14709 = CARTESIAN_POINT ( 'NONE',  ( 43.81606138205700063, 3.151453266960317023, 6.397347472316774031 ) ) ;
#14710 = FILL_AREA_STYLE_COLOUR ( '', #25131 ) ;
#14711 = CARTESIAN_POINT ( 'NONE',  ( 40.14115730948191185, -18.51368208888610667, 71.32335560751960202 ) ) ;
#14712 = LINE ( 'NONE', #3375, #10082 ) ;
#14713 = DIRECTION ( 'NONE',  ( 0.000000000000000000, 0.000000000000000000, -1.000000000000000000 ) ) ;
#14714 = VECTOR ( 'NONE', #22114, 1000.000000000000000 ) ;
#14715 = EDGE_LOOP ( 'NONE', ( #14873, #15316, #24345, #12725 ) ) ;
#14716 = AXIS2_PLACEMENT_3D ( 'NONE', #12297, #20266, #11917 ) ;
#14717 = VECTOR ( 'NONE', #23525, 1000.000000000000114 ) ;
#14718 = CARTESIAN_POINT ( 'NONE',  ( 32.81606138205700773, 2.740850673309605412, 6.112030963703427133 ) ) ;
#14719 = PLANE ( 'NONE',  #23333 ) ;
#14720 = CARTESIAN_POINT ( 'NONE',  ( 39.82603832034401137, -13.30384086642190589, 70.35351908239857721 ) ) ;
#14721 = DIRECTION ( 'NONE',  ( 1.000000000000000000, 0.000000000000000000, 0.000000000000000000 ) ) ;
#14722 = DIRECTION ( 'NONE',  ( -1.000000000000000000, 5.510910596163088391E-31, 1.836970198721029688E-16 ) ) ;
#14723 = CARTESIAN_POINT ( 'NONE',  ( 38.37017380507020192, -28.01368208888610667, 73.11602215082115208 ) ) ;
#14724 = ORIENTED_EDGE ( 'NONE', *, *, #17841, .T. ) ;
#14725 = LINE ( 'NONE', #22712, #25013 ) ;
#14726 = EDGE_CURVE ( 'NONE', #10123, #24470, #15299, .T. ) ;
#14727 = DIRECTION ( 'NONE',  ( -1.000000000000000000, 1.115179377413661005E-30, 3.717264591378870232E-16 ) ) ;
#14728 = CARTESIAN_POINT ( 'NONE',  ( 37.69796330110505522, -26.50384086642190695, 73.09843995877328382 ) ) ;
#14729 = CARTESIAN_POINT ( 'NONE',  ( 36.31606138205700063, -20.32127907754186680, 75.99695190479390305 ) ) ;
#14730 = CARTESIAN_POINT ( 'NONE',  ( 38.37017380507020192, -22.01368208888611022, 73.11602215082116629 ) ) ;
#14731 = EDGE_LOOP ( 'NONE', ( #11051, #21985, #13240, #3691 ) ) ;
#14732 = ORIENTED_EDGE ( 'NONE', *, *, #17892, .T. ) ;
#14733 = CARTESIAN_POINT ( 'NONE',  ( 40.06606138205700063, 6.004618353093779781, 2.291321535809666354 ) ) ;
#14734 = CARTESIAN_POINT ( 'NONE',  ( 38.41621794735363693, -36.60729675983900222, 84.30501292737011454 ) ) ;
#14735 = SHAPE_REPRESENTATION ( 'Upper Metal Lever Arm', ( #2000 ), #3041 ) ;
#14736 = CARTESIAN_POINT ( 'NONE',  ( 38.93987200065208754, 1.186317911113898838, 70.42958956619170863 ) ) ;
#14737 = AXIS2_PLACEMENT_3D ( 'NONE', #23117, #22995, #19518 ) ;
#14738 = CARTESIAN_POINT ( 'NONE',  ( 38.93987200065210175, -28.80384086642191477, 72.33091598616823603 ) ) ;
#14739 = ORIENTED_EDGE ( 'NONE', *, *, #11713, .T. ) ;
#14740 = ORIENTED_EDGE ( 'NONE', *, *, #14927, .T. ) ;
#14741 = CARTESIAN_POINT ( 'NONE',  ( 36.06606138205700063, 5.594015759443068170, 2.006005027196319901 ) ) ;
#14742 = ORIENTED_EDGE ( 'NONE', *, *, #198, .F. ) ;
#14743 = SURFACE_STYLE_USAGE ( .BOTH. , #12957 ) ;
#14744 = CARTESIAN_POINT ( 'NONE',  ( 37.69796330110505522, -4.503840866421913169, 73.09843995877331224 ) ) ;
#14745 = ADVANCED_FACE ( 'NONE', ( #6798 ), #849, .T. ) ;
#14746 = CARTESIAN_POINT ( 'NONE',  ( 45.81606138205697221, -4.589472609077215104, -6.350807634294793225 ) ) ;
#14747 = EDGE_CURVE ( 'NONE', #15899, #15633, #16317, .T. ) ;
#14748 = CARTESIAN_POINT ( 'NONE',  ( 40.31606138205700773, -10.66749763588699906, 14.47455635838400134 ) ) ;
#14749 = EDGE_CURVE ( 'NONE', #3879, #22990, #10672, .T. ) ;
#14750 = ORIENTED_EDGE ( 'NONE', *, *, #10524, .F. ) ;
#14751 = VERTEX_POINT ( 'NONE', #18518 ) ;
#14752 = EDGE_CURVE ( 'NONE', #17171, #6977, #2964, .T. ) ;
#14753 = PRESENTATION_LAYER_ASSIGNMENT (  '', '', ( #22987 ) ) ;
#14754 = ADVANCED_FACE ( 'NONE', ( #25050 ), #24542, .T. ) ;
#14755 = ORIENTED_EDGE ( 'NONE', *, *, #12189, .T. ) ;
#14756 = CYLINDRICAL_SURFACE ( 'NONE', #21929, 2.000000000000001776 ) ;
#14757 = CARTESIAN_POINT ( 'NONE',  ( 39.95015449827720744, 1.386317911113894130, 70.79240656858108593 ) ) ;
#14758 = CARTESIAN_POINT ( 'NONE',  ( 35.31606138205700773, 1.535676793533870210, 63.36117568837578062 ) ) ;
#14759 = DIRECTION ( 'NONE',  ( 0.000000000000000000, 0.8212051873014210024, 0.5706330172266920187 ) ) ;
#14760 = AXIS2_PLACEMENT_3D ( 'NONE', #8179, #17719, #4320 ) ;
#14761 = CARTESIAN_POINT ( 'NONE',  ( 36.31606138205697931, -5.528433326023629135, -4.448224773462933435 ) ) ;
#14762 = EDGE_CURVE ( 'NONE', #23854, #24510, #4990, .T. ) ;
#14763 = DIRECTION ( 'NONE',  ( -0.000000000000000000, -0.7540134720837717852, -0.6568589528324747517 ) ) ;
#14764 = LINE ( 'NONE', #20564, #5744 ) ;
#14765 = CARTESIAN_POINT ( 'NONE',  ( 40.31606138205700773, -20.22127907754186893, 75.50705395623725735 ) ) ;
#14766 = CIRCLE ( 'NONE', #22171, 1.499999999999994005 ) ;
#14767 = DIRECTION ( 'NONE',  ( 1.000000000000000000, 1.817449160981365809E-30, -1.734723475976805122E-15 ) ) ;
#14768 = ORIENTED_EDGE ( 'NONE', *, *, #4846, .T. ) ;
#14769 = VERTEX_POINT ( 'NONE', #16841 ) ;
#14770 = CARTESIAN_POINT ( 'NONE',  ( 36.31606138205700063, -12.97731741051368282, 21.08248588348817876 ) ) ;
#14771 = AXIS2_PLACEMENT_3D ( 'NONE', #3223, #18956, #20885 ) ;
#14772 = DIRECTION ( 'NONE',  ( 1.000000000000000000, 0.000000000000000000, -0.000000000000000000 ) ) ;
#14773 = CARTESIAN_POINT ( 'NONE',  ( 37.69225076346193504, -17.81368208888610383, 72.33091598616826445 ) ) ;
#14774 = ORIENTED_EDGE ( 'NONE', *, *, #23265, .F. ) ;
#14775 = ORIENTED_EDGE ( 'NONE', *, *, #1387, .F. ) ;
#14776 = DIRECTION ( 'NONE',  ( 1.000000000000000000, -5.204170427930413121E-31, -1.734723475976804876E-16 ) ) ;
#14777 = CARTESIAN_POINT ( 'NONE',  ( 38.26194895904383486, -5.013682088886102228, 69.64448340153879258 ) ) ;
#14778 = CARTESIAN_POINT ( 'NONE',  ( 40.14115730948191185, -25.10384086642190482, 71.43714994484028580 ) ) ;
#14779 = VECTOR ( 'NONE', #13943, 1000.000000000000000 ) ;
#14780 = DIRECTION ( 'NONE',  ( 1.327674326049719602E-15, -0.4425581086832399147, 0.8967398287344627850 ) ) ;
#14781 = CARTESIAN_POINT ( 'NONE',  ( 36.89935272106204422, -9.213682088886100630, 69.52238214136768590 ) ) ;
#14782 = EDGE_CURVE ( 'NONE', #11945, #23547, #22634, .T. ) ;
#14783 = AXIS2_PLACEMENT_3D ( 'NONE', #6024, #9767, #4094 ) ;
#14784 = CYLINDRICAL_SURFACE ( 'NONE', #15423, 1.500000000000001332 ) ;
#14785 = ADVANCED_FACE ( 'NONE', ( #5248 ), #17227, .T. ) ;
#14786 = CARTESIAN_POINT ( 'NONE',  ( 40.31606138205700773, -7.204193249396275256, 83.11277699141410835 ) ) ;
#14787 = CARTESIAN_POINT ( 'NONE',  ( 41.31606138205687273, 43.19123852234596939, 65.30501292736988717 ) ) ;
#14788 = LINE ( 'NONE', #20722, #20678 ) ;
#14789 = VECTOR ( 'NONE', #4353, 1000.000000000000000 ) ;
#14790 = CARTESIAN_POINT ( 'NONE',  ( 39.91050633825327054, -5.951964217243578048, 82.77254663560049153 ) ) ;
#14791 = DIRECTION ( 'NONE',  ( -1.734723475976804876E-16, 1.000000000000000000, 0.000000000000000000 ) ) ;
#14792 = DIRECTION ( 'NONE',  ( -1.734723475976804876E-16, -3.469446951953610245E-15, -1.000000000000000000 ) ) ;
#14793 = VECTOR ( 'NONE', #12060, 1000.000000000000000 ) ;
#14794 = ORIENTED_EDGE ( 'NONE', *, *, #23908, .T. ) ;
#14795 = LINE ( 'NONE', #1508, #24652 ) ;
#14796 = DIRECTION ( 'NONE',  ( 1.000000000000000000, 0.000000000000000000, 0.000000000000000000 ) ) ;
#14797 = EDGE_LOOP ( 'NONE', ( #925, #18975, #24889, #18619 ) ) ;
#14798 = ORIENTED_EDGE ( 'NONE', *, *, #5157, .F. ) ;
#14799 = CARTESIAN_POINT ( 'NONE',  ( 37.50301148336529877, -18.50384086642192116, 73.69843995877327814 ) ) ;
#14800 = AXIS2_PLACEMENT_3D ( 'NONE', #1460, #14858, #20800 ) ;
#14801 = ADVANCED_FACE ( 'NONE', ( #15031 ), #6923, .T. ) ;
#14802 = CARTESIAN_POINT ( 'NONE',  ( 38.37017380507020192, -20.01368208888610667, 73.11602215082116629 ) ) ;
#14803 = DIRECTION ( 'NONE',  ( -1.000000000000000000, -2.751104698760144965E-15, 1.228345504986737969E-16 ) ) ;
#14804 = DIRECTION ( 'NONE',  ( -8.791731484610113542E-17, 0.9135454576426023099, 0.4067366430757970996 ) ) ;
#14805 = ORIENTED_EDGE ( 'NONE', *, *, #9282, .F. ) ;
#14806 = CARTESIAN_POINT ( 'NONE',  ( 43.81606138205700063, 41.44123852234597649, 67.80501292736988717 ) ) ;
#14807 = PLANE ( 'NONE',  #17425 ) ;
#14808 = CARTESIAN_POINT ( 'NONE',  ( 39.12911128074872380, 0.4961591335780889955, 69.06206559358666652 ) ) ;
#14809 = ORIENTED_EDGE ( 'NONE', *, *, #2407, .T. ) ;
#14810 = FACE_BOUND ( 'NONE', #20425, .T. ) ;
#14811 = CARTESIAN_POINT ( 'NONE',  ( 43.81606138205700063, 36.92314894770294131, 80.37823623207323465 ) ) ;
#14812 = CARTESIAN_POINT ( 'NONE',  ( 36.87297107704152666, -1.713682088886108179, 72.49904802271743165 ) ) ;
#14813 = DIRECTION ( 'NONE',  ( 0.000000000000000000, -1.387778780781454037E-14, 1.000000000000000000 ) ) ;
#14814 = CARTESIAN_POINT ( 'NONE',  ( 37.25202387243752611, -21.21368208888610241, 70.00779233799262613 ) ) ;
#14815 = VECTOR ( 'NONE', #12665, 1000.000000000000000 ) ;
#14816 = CARTESIAN_POINT ( 'NONE',  ( 45.81606138205697221, -4.589472609077215992, -6.350807634294792337 ) ) ;
#14817 = DIRECTION ( 'NONE',  ( -0.000000000000000000, -3.469446951953613400E-15, -1.000000000000000000 ) ) ;
#14818 = AXIS2_PLACEMENT_3D ( 'NONE', #18416, #16464, #20217 ) ;
#14819 = CARTESIAN_POINT ( 'NONE',  ( 39.24876120206129571, -20.90384086642191264, 72.12822762946747446 ) ) ;
#14820 = CARTESIAN_POINT ( 'NONE',  ( 37.33957961208646736, -5.813682088886107380, 72.81632618279323310 ) ) ;
#14821 = CARTESIAN_POINT ( 'NONE',  ( 39.54692359221319009, -21.81983708080221973, 75.31129620181626194 ) ) ;
#14822 = EDGE_LOOP ( 'NONE', ( #23501, #896, #6784, #10525 ) ) ;
#14823 = EDGE_CURVE ( 'NONE', #18487, #2496, #14900, .T. ) ;
#14824 = CARTESIAN_POINT ( 'NONE',  ( 36.64852494920107517, -2.203840866421912015, 71.86517103874049894 ) ) ;
#14825 = CARTESIAN_POINT ( 'NONE',  ( 36.31606138205700063, -14.15704008206721909, 14.73030834591676808 ) ) ;
#14826 = EDGE_CURVE ( 'NONE', #20085, #2367, #1246, .T. ) ;
#14827 = CARTESIAN_POINT ( 'NONE',  ( 38.82593461698262871, -2.913682088886099919, 69.62690120949091011 ) ) ;
#14828 = ORIENTED_EDGE ( 'NONE', *, *, #2586, .T. ) ;
#14829 = CARTESIAN_POINT ( 'NONE',  ( 37.61123632939165873, -7.913682088886107913, 73.73360434286902887 ) ) ;
#14830 = ORIENTED_EDGE ( 'NONE', *, *, #141, .F. ) ;
#14831 = FACE_OUTER_BOUND ( 'NONE', #3849, .T. ) ;
#14832 = CARTESIAN_POINT ( 'NONE',  ( 38.63098279924290068, -14.70384086642191157, 72.53360434286904024 ) ) ;
#14833 = CARTESIAN_POINT ( 'NONE',  ( 38.31606138205700063, -4.070846987468769385, 59.14016975459033887 ) ) ;
#14834 = AXIS2_PLACEMENT_3D ( 'NONE', #8893, #2937, #24448 ) ;
#14835 = ORIENTED_EDGE ( 'NONE', *, *, #1513, .F. ) ;
#14836 = FACE_OUTER_BOUND ( 'NONE', #17024, .T. ) ;
#14837 = DIRECTION ( 'NONE',  ( -1.734723475976804876E-16, -3.269436733918100469E-15, -1.000000000000000000 ) ) ;
#14838 = CARTESIAN_POINT ( 'NONE',  ( 37.61123632939164452, -13.70384086642191157, 69.02690120949091579 ) ) ;
#14839 = CIRCLE ( 'NONE', #18151, 1.999999999999997113 ) ;
#14840 = CARTESIAN_POINT ( 'NONE',  ( 36.57656417722905928, -21.26713369642283524, 75.85247656039494757 ) ) ;
#14841 = CARTESIAN_POINT ( 'NONE',  ( 36.68196826583682935, -21.61368208888610454, 71.96809898377888715 ) ) ;
#14842 = CARTESIAN_POINT ( 'NONE',  ( 47.81606138205697221, -29.47337283097070326, 44.07055847651734837 ) ) ;
#14843 = DIRECTION ( 'NONE',  ( -1.000000000000000000, 5.204170427930415223E-30, 1.734723475976805122E-15 ) ) ;
#14844 = EDGE_LOOP ( 'NONE', ( #3427, #16407, #17410 ) ) ;
#14845 = FACE_OUTER_BOUND ( 'NONE', #17343, .T. ) ;
#14846 = PLANE ( 'NONE',  #6488 ) ;
#14847 = CARTESIAN_POINT ( 'NONE',  ( 39.82603832034401137, -7.303840866421907663, 70.35351908239860563 ) ) ;
#14848 = PRODUCT_CONTEXT ( 'NONE', #13591, 'mechanical' ) ;
#14849 = DIRECTION ( 'NONE',  ( 0.000000000000000000, -1.000000000000000000, 2.999999999999999839E-15 ) ) ;
#14850 = CARTESIAN_POINT ( 'NONE',  ( 38.93415946300897446, -24.11368208888610454, 73.09843995877328382 ) ) ;
#14851 = PLANE ( 'NONE',  #1175 ) ;
#14852 = CIRCLE ( 'NONE', #6642, 0.5000000000000004441 ) ;
#14853 = CARTESIAN_POINT ( 'NONE',  ( 39.98359781491296161, -25.20384086642191335, 70.89533451361944572 ) ) ;
#14854 = CARTESIAN_POINT ( 'NONE',  ( 36.57656417722905928, -21.26713369642283880, 75.85247656039494757 ) ) ;
#14855 = CARTESIAN_POINT ( 'NONE',  ( 36.68196826583682935, -21.61368208888610454, 71.96809898377888715 ) ) ;
#14856 = VERTEX_POINT ( 'NONE', #3175 ) ;
#14857 = EDGE_LOOP ( 'NONE', ( #18606, #5156, #7849, #12444 ) ) ;
#14858 = DIRECTION ( 'NONE',  ( 1.000000000000000000, 1.000000000000000078E-15, 0.000000000000000000 ) ) ;
#14859 = CARTESIAN_POINT ( 'NONE',  ( 34.81606138205687273, 43.19123852234595518, 61.30501292736988006 ) ) ;
#14860 = CARTESIAN_POINT ( 'NONE',  ( 38.63098279924290068, -28.70384086642190979, 72.53360434286901182 ) ) ;
#14861 = CARTESIAN_POINT ( 'NONE',  ( 39.41296390513587511, 1.586317911113900081, 71.67976084211552745 ) ) ;
#14862 = EDGE_LOOP ( 'NONE', ( #15463, #19302, #563, #471 ) ) ;
#14863 = VERTEX_POINT ( 'NONE', #18772 ) ;
#14864 = LINE ( 'NONE', #22726, #21982 ) ;
#14865 = CARTESIAN_POINT ( 'NONE',  ( 43.69896204258590444, 3.548173818309682037, 6.215045287937394747 ) ) ;
#14866 = ORIENTED_EDGE ( 'NONE', *, *, #9499, .F. ) ;
#14867 = CARTESIAN_POINT ( 'NONE',  ( 33.31606138205700773, 0.9984178969752143251, 11.59873562314662010 ) ) ;
#14868 = CARTESIAN_POINT ( 'NONE',  ( 38.93415946300896024, -5.503840866421906952, 69.66206559358663242 ) ) ;
#14869 = LINE ( 'NONE', #3528, #8000 ) ;
#14870 = ADVANCED_FACE ( 'NONE', ( #22760 ), #7184, .T. ) ;
#14871 = DIRECTION ( 'NONE',  ( 0.000000000000000000, 0.000000000000000000, 1.000000000000000000 ) ) ;
#14872 = ORIENTED_EDGE ( 'NONE', *, *, #22638, .F. ) ;
#14873 = ORIENTED_EDGE ( 'NONE', *, *, #22810, .F. ) ;
#14874 = ORIENTED_EDGE ( 'NONE', *, *, #10716, .T. ) ;
#14875 = CARTESIAN_POINT ( 'NONE',  ( 43.81606138205700063, 2.191238522347013440, 73.80501292737000085 ) ) ;
#14876 = CARTESIAN_POINT ( 'NONE',  ( 37.33957961208646736, -3.813682088886109156, 72.81632618279323310 ) ) ;
#14877 = COLOUR_RGB ( '', 0.66274510, 0.83137255, 0.94901961) ;
#14878 = LINE ( 'NONE', #963, #8576 ) ;
#14879 = PLANE ( 'NONE',  #6688 ) ;
#14880 = ORIENTED_EDGE ( 'NONE', *, *, #1124, .F. ) ;
#14881 = DIRECTION ( 'NONE',  ( -1.000000000000000000, -1.734723475976804876E-16, 1.734723475976814737E-16 ) ) ;
#14882 = CARTESIAN_POINT ( 'NONE',  ( 42.96606138205698500, -7.467730535347522292, -2.778285769174305919 ) ) ;
#14883 = DIRECTION ( 'NONE',  ( 1.000000000000000000, 0.000000000000000000, 0.000000000000000000 ) ) ;
#14884 = CARTESIAN_POINT ( 'NONE',  ( 37.68611352887096189, -5.296788164819011158, 82.80469560528126749 ) ) ;
#14886 = ADVANCED_FACE ( 'NONE', ( #16970 ), #15283, .T. ) ;
#14885 = SURFACE_STYLE_USAGE ( .BOTH. , #22877 ) ;
#14887 = ADVANCED_FACE ( 'NONE', ( #3045 ), #5127, .F. ) ;
#14888 = VECTOR ( 'NONE', #14588, 1000.000000000000000 ) ;
#14889 = CARTESIAN_POINT ( 'NONE',  ( 35.64099152588522657, -8.607181138186998481, 79.30501292737000085 ) ) ;
#14890 = ORIENTED_EDGE ( 'NONE', *, *, #25099, .T. ) ;
#14891 = ORIENTED_EDGE ( 'NONE', *, *, #14599, .T. ) ;
#14892 = DIRECTION ( 'NONE',  ( -7.071067811865491110E-16, 0.9008287146801832179, -0.4341746501209495790 ) ) ;
#14893 = CARTESIAN_POINT ( 'NONE',  ( 43.81606138205700063, -34.55876147765400930, 73.55501292737011454 ) ) ;
#14894 = EDGE_CURVE ( 'NONE', #12758, #9931, #24676, .T. ) ;
#14895 =( REPRESENTATION_RELATIONSHIP ('NONE','NONE', #17377, #4169 ) REPRESENTATION_RELATIONSHIP_WITH_TRANSFORMATION ( #19475 )SHAPE_REPRESENTATION_RELATIONSHIP( ) );
#14896 = CARTESIAN_POINT ( 'NONE',  ( 39.31564783533280405, -16.31368208888610383, 72.03616607671141026 ) ) ;
#14897 = ORIENTED_EDGE ( 'NONE', *, *, #6170, .F. ) ;
#14898 = ORIENTED_EDGE ( 'NONE', *, *, #6032, .T. ) ;
#14899 = VECTOR ( 'NONE', #1144, 1000.000000000000000 ) ;
#14900 = LINE ( 'NONE', #3553, #14914 ) ;
#14901 = CARTESIAN_POINT ( 'NONE',  ( 36.68196826583682935, -3.613682088886103205, 71.96809898377890136 ) ) ;
#14902 = CARTESIAN_POINT ( 'NONE',  ( 37.69796330110505522, -24.50384086642190695, 73.09843995877328382 ) ) ;
#14903 = CARTESIAN_POINT ( 'NONE',  ( 36.81465384343994884, 40.76768529863396395, 79.57823623207323749 ) ) ;
#14904 = EDGE_CURVE ( 'NONE', #24509, #6270, #11181, .T. ) ;
#14905 = CARTESIAN_POINT ( 'NONE',  ( 36.36258059203031934, -9.713682088886105959, 72.86986841596736042 ) ) ;
#14906 = FACE_OUTER_BOUND ( 'NONE', #13075, .T. ) ;
#14907 = ORIENTED_EDGE ( 'NONE', *, *, #1300, .T. ) ;
#14908 = FACE_OUTER_BOUND ( 'NONE', #24118, .T. ) ;
#14909 = CARTESIAN_POINT ( 'NONE',  ( 33.63430007298546087, 2.841684771932709186, 6.101742786271089791 ) ) ;
#14910 = AXIS2_PLACEMENT_3D ( 'NONE', #13496, #21228, #2015 ) ;
#14911 = CARTESIAN_POINT ( 'NONE',  ( 35.31606138205687273, 33.19123852234596939, 65.30501292736991559 ) ) ;
#14912 = CARTESIAN_POINT ( 'NONE',  ( 38.31606138205700063, -5.204193249396280585, 82.80001292736993435 ) ) ;
#14913 = DIRECTION ( 'NONE',  ( -2.994052579541399595E-16, 1.632680918566405413E-15, -1.000000000000000000 ) ) ;
#14914 = VECTOR ( 'NONE', #12856, 1000.000000000000114 ) ;
#14915 = CARTESIAN_POINT ( 'NONE',  ( 32.81606138205700773, 6.705285648480822758, 7.416521610403067122 ) ) ;
#14916 = EDGE_CURVE ( 'NONE', #11164, #11722, #21767, .T. ) ;
#14917 = ORIENTED_EDGE ( 'NONE', *, *, #5824, .T. ) ;
#14918 = EDGE_CURVE ( 'NONE', #12986, #19369, #23553, .T. ) ;
#14919 = DIRECTION ( 'NONE',  ( 0.000000000000000000, -1.000000000000000000, 2.999999999999999839E-15 ) ) ;
#14920 = AXIS2_PLACEMENT_3D ( 'NONE', #25346, #14408, #17906 ) ;
#14921 = DIRECTION ( 'NONE',  ( -2.690219486203388234E-15, 0.8967398287344627850, 0.4425581086832399147 ) ) ;
#14922 = ORIENTED_EDGE ( 'NONE', *, *, #4836, .T. ) ;
#14923 = AXIS2_PLACEMENT_3D ( 'NONE', #22387, #14529, #12615 ) ;
#14924 = ADVANCED_FACE ( 'NONE', ( #21093, #13242 ), #3438, .F. ) ;
#14925 = VERTEX_POINT ( 'NONE', #15418 ) ;
#14926 = CARTESIAN_POINT ( 'NONE',  ( 36.89935272106205133, -16.40384086642191974, 73.23812341099225875 ) ) ;
#14927 = EDGE_CURVE ( 'NONE', #467, #3314, #23512, .T. ) ;
#14928 = EDGE_CURVE ( 'NONE', #13108, #17733, #17389, .T. ) ;
#14929 = CIRCLE ( 'NONE', #23566, 1.750000000000001554 ) ;
#14930 = CARTESIAN_POINT ( 'NONE',  ( 36.64852494920107517, -23.41368208888610525, 70.89533451361945993 ) ) ;
#14931 = CARTESIAN_POINT ( 'NONE',  ( 44.81606138205700063, -34.55876147765400930, 73.30501292737011454 ) ) ;
#14932 = VECTOR ( 'NONE', #12597, 1000.000000000000000 ) ;
#14933 = VERTEX_POINT ( 'NONE', #19658 ) ;
#14934 = CARTESIAN_POINT ( 'NONE',  ( 32.81606138205700773, -20.88462213363798270, 44.49284693533410717 ) ) ;
#14935 = DIRECTION ( 'NONE',  ( 1.000000000000000000, 0.000000000000000000, -1.734723475976814737E-16 ) ) ;
#14936 = VECTOR ( 'NONE', #15632, 1000.000000000000000 ) ;
#14937 = EDGE_CURVE ( 'NONE', #5642, #22433, #9583, .T. ) ;
#14938 = CARTESIAN_POINT ( 'NONE',  ( 35.86008812008917346, -25.51368208888610667, 71.43714994484032843 ) ) ;
#14939 = EDGE_CURVE ( 'NONE', #8708, #21114, #21465, .T. ) ;
#14940 = ORIENTED_EDGE ( 'NONE', *, *, #1676, .F. ) ;
#14941 = DIRECTION ( 'NONE',  ( -2.792262043613788535E-15, 0.8967398287344627850, 0.4425581086832399147 ) ) ;
#14942 = DIRECTION ( 'NONE',  ( 1.000000000000000000, 0.000000000000000000, 0.000000000000000000 ) ) ;
#14943 = CARTESIAN_POINT ( 'NONE',  ( 37.33957961208646736, -1.813682088886107380, 72.81632618279323310 ) ) ;
#14944 = PLANE ( 'NONE',  #11406 ) ;
#14945 = VECTOR ( 'NONE', #2136, 1000.000000000000114 ) ;
#14946 = CARTESIAN_POINT ( 'NONE',  ( 38.93415946300898867, -20.11368208888610809, 73.09843995877329803 ) ) ;
#14947 = LINE ( 'NONE', #15069, #25022 ) ;
#14948 = EDGE_CURVE ( 'NONE', #16335, #1085, #15913, .T. ) ;
#14949 = AXIS2_PLACEMENT_3D ( 'NONE', #11262, #17053, #18980 ) ;
#14950 = CARTESIAN_POINT ( 'NONE',  ( 46.81606138205696510, -3.028410647649130816, 0.3252050635115383281 ) ) ;
#14951 = CARTESIAN_POINT ( 'NONE',  ( 39.37952058850012804, -19.00384086642191406, 71.78268878715390144 ) ) ;
#14952 = CARTESIAN_POINT ( 'NONE',  ( 37.69796330110504101, -7.113682088886100985, 69.66206559358663242 ) ) ;
#14953 = VERTEX_POINT ( 'NONE', #17607 ) ;
#14954 = DIRECTION ( 'NONE',  ( -3.717264591378870232E-16, -2.999999999999999839E-15, -1.000000000000000000 ) ) ;
#14955 = AXIS2_PLACEMENT_3D ( 'NONE', #10706, #4762, #2691 ) ;
#14956 = ORIENTED_EDGE ( 'NONE', *, *, #8386, .F. ) ;
#14957 = CARTESIAN_POINT ( 'NONE',  ( 37.33957961208645315, -5.803840866421907663, 69.94417936956673998 ) ) ;
#14958 = CARTESIAN_POINT ( 'NONE',  ( 38.31606138205700063, 16.19123852234700678, 71.30501292736995822 ) ) ;
#14959 = CARTESIAN_POINT ( 'NONE',  ( 36.68196826583682935, -1.613682088886104982, 71.96809898377890136 ) ) ;
#14960 = ORIENTED_EDGE ( 'NONE', *, *, #17941, .F. ) ;
#14961 = CARTESIAN_POINT ( 'NONE',  ( 40.52078840805428683, -8.613682088886102761, 70.60699637195608602 ) ) ;
#14962 = EDGE_LOOP ( 'NONE', ( #11958, #16123, #14486, #12880, #13027, #3690, #1280, #2049 ) ) ;
#14963 = FACE_OUTER_BOUND ( 'NONE', #21368, .T. ) ;
#14964 = CARTESIAN_POINT ( 'NONE',  ( 37.60469502381300799, -14.40384086642191441, 72.26730301774234988 ) ) ;
#14965 =( GEOMETRIC_REPRESENTATION_CONTEXT ( 3 ) GLOBAL_UNCERTAINTY_ASSIGNED_CONTEXT ( ( #12629 ) ) GLOBAL_UNIT_ASSIGNED_CONTEXT ( ( #1909, #19570, #17525 ) ) REPRESENTATION_CONTEXT ( 'NONE', 'WORKASPACE' ) );
#14966 = CARTESIAN_POINT ( 'NONE',  ( 44.81606138205700063, 39.39281886181299797, 81.75501292736983316 ) ) ;
#14967 = ORIENTED_EDGE ( 'NONE', *, *, #10564, .F. ) ;
#14968 = CARTESIAN_POINT ( 'NONE',  ( 44.81606138205700063, 38.19123852234598360, 71.05501292736988717 ) ) ;
#14969 = CARTESIAN_POINT ( 'NONE',  ( 35.31606138205687273, 33.19123852234596939, 65.30501292736991559 ) ) ;
#14970 = CARTESIAN_POINT ( 'NONE',  ( 39.64521430340305841, -18.80384086642191477, 73.30173637941818754 ) ) ;
#14971 = AXIS2_PLACEMENT_3D ( 'NONE', #14036, #6182, #1912 ) ;
#14972 = CARTESIAN_POINT ( 'NONE',  ( 37.66883992158368955, -22.11812637443705043, 75.30036834061758100 ) ) ;
#14973 = DIRECTION ( 'NONE',  ( -1.156482317317871478E-16, -0.4425581086832399147, 0.8967398287344627850 ) ) ;
#14974 = CARTESIAN_POINT ( 'NONE',  ( 37.25202387243752611, -23.21368208888610241, 70.00779233799262613 ) ) ;
#14975 = DIRECTION ( 'NONE',  ( -2.727049986597863807E-15, 0.7516416929448760387, 0.6595716529892418079 ) ) ;
#14976 = VECTOR ( 'NONE', #4464, 1000.000000000000000 ) ;
#14977 = LINE ( 'NONE', #14469, #15145 ) ;
#14978 = EDGE_CURVE ( 'NONE', #8428, #22767, #25436, .T. ) ;
#14979 = VERTEX_POINT ( 'NONE', #5881 ) ;
#14980 = EDGE_CURVE ( 'NONE', #13361, #9366, #8752, .T. ) ;
#14981 = DIRECTION ( 'NONE',  ( 1.000000000000000000, -0.000000000000000000, 0.000000000000000000 ) ) ;
#14982 = FACE_OUTER_BOUND ( 'NONE', #8033, .T. ) ;
#14983 = CARTESIAN_POINT ( 'NONE',  ( 37.25202387243754032, -10.40384086642191441, 72.75271321436733274 ) ) ;
#14984 = DIRECTION ( 'NONE',  ( 1.000000000000000000, -0.000000000000000000, 0.000000000000000000 ) ) ;
#14985 = CARTESIAN_POINT ( 'NONE',  ( 37.33957961208646736, -21.81368208888610738, 72.81632618279321889 ) ) ;
#14986 = PRODUCT_DEFINITION_FORMATION_WITH_SPECIFIED_SOURCE ( 'ANY', '', #2305, .NOT_KNOWN. ) ;
#14987 = DIRECTION ( 'NONE',  ( 0.000000000000000000, -0.6568589528324746407, 0.7540134720837717852 ) ) ;
#14988 = AXIS2_PLACEMENT_3D ( 'NONE', #24227, #20005, #24105 ) ;
#14989 = CARTESIAN_POINT ( 'NONE',  ( 39.82603832034400426, -25.30384086642190766, 70.35351908239857721 ) ) ;
#14990 = CARTESIAN_POINT ( 'NONE',  ( 37.09113907096683960, -21.82847486639043311, 75.81287845682257398 ) ) ;
#14991 = AXIS2_PLACEMENT_3D ( 'NONE', #25281, #23355, #17707 ) ;
#14992 = CARTESIAN_POINT ( 'NONE',  ( 37.69796330110504101, -25.11368208888609388, 69.66206559358660400 ) ) ;
#14993 = ORIENTED_EDGE ( 'NONE', *, *, #17309, .F. ) ;
#14994 = VERTEX_POINT ( 'NONE', #13485 ) ;
#14995 = LINE ( 'NONE', #17067, #3267 ) ;
#14996 = CYLINDRICAL_SURFACE ( 'NONE', #24787, 0.7500000000000008882 ) ;
#14997 = CARTESIAN_POINT ( 'NONE',  ( 38.00113996487114321, 0.08631791111389855442, 72.53360434286905445 ) ) ;
#14998 = EDGE_LOOP ( 'NONE', ( #15690, #18751, #8672, #25145 ) ) ;
#14999 = EDGE_LOOP ( 'NONE', ( #18148, #6778, #18998, #20861 ) ) ;
#15000 = CARTESIAN_POINT ( 'NONE',  ( 45.81606138205707168, -38.42645682328033985, 63.90656833300437256 ) ) ;
#15001 = FACE_OUTER_BOUND ( 'NONE', #4923, .T. ) ;
#15002 = ORIENTED_EDGE ( 'NONE', *, *, #3996, .T. ) ;
#15003 = FACE_OUTER_BOUND ( 'NONE', #10614, .T. ) ;
#15004 = CARTESIAN_POINT ( 'NONE',  ( 40.14115730948191185, -5.103840866421909261, 71.43714994484034264 ) ) ;
#15005 = CARTESIAN_POINT ( 'NONE',  ( 43.06606138205700063, -34.55876147765400930, 73.55501292737011454 ) ) ;
#15006 = DIRECTION ( 'NONE',  ( 0.000000000000000000, -0.8212051873014210024, -0.5706330172266920187 ) ) ;
#15007 = VERTEX_POINT ( 'NONE', #1996 ) ;
#15008 = EDGE_LOOP ( 'NONE', ( #4085, #53, #6730, #701 ) ) ;
#15009 = ADVANCED_FACE ( 'NONE', ( #8074 ), #13744, .T. ) ;
#15010 = VERTEX_POINT ( 'NONE', #21335 ) ;
#15011 = ADVANCED_FACE ( 'NONE', ( #25176 ), #39, .T. ) ;
#15012 = DIRECTION ( 'NONE',  ( -1.000000000000000000, -2.999999999999999839E-15, 0.000000000000000000 ) ) ;
#15013 = CARTESIAN_POINT ( 'NONE',  ( 39.98359781491296161, -2.413682088886103472, 71.86517103874048473 ) ) ;
#15014 = CARTESIAN_POINT ( 'NONE',  ( 44.81606138205700063, 35.44123852234597649, 67.80501292736990138 ) ) ;
#15015 = CARTESIAN_POINT ( 'NONE',  ( 34.66606138205693810, 5.651448314156965580, 4.532640732625139002 ) ) ;
#15016 = ORIENTED_EDGE ( 'NONE', *, *, #1316, .T. ) ;
#15017 = CARTESIAN_POINT ( 'NONE',  ( 33.31606138205700773, -21.26162886970023536, 44.16441745890789150 ) ) ;
#15018 = CARTESIAN_POINT ( 'NONE',  ( 30.81606138205697576, -4.349482454670884124, -5.142398479549302515 ) ) ;
#15019 = LINE ( 'NONE', #16561, #16854 ) ;
#15020 = CARTESIAN_POINT ( 'NONE',  ( 34.06606138205700773, -32.75315594507191008, 59.38245422252773409 ) ) ;
#15021 = ADVANCED_FACE ( 'NONE', ( #19402 ), #21599, .F. ) ;
#15022 = DIRECTION ( 'NONE',  ( 9.027796614315171564E-31, 1.000000000000000000, 1.163336342344335610E-15 ) ) ;
#15023 = ORIENTED_EDGE ( 'NONE', *, *, #11687, .T. ) ;
#15024 = ORIENTED_EDGE ( 'NONE', *, *, #11980, .F. ) ;
#15025 = VECTOR ( 'NONE', #18051, 1000.000000000000000 ) ;
#15026 = DIRECTION ( 'NONE',  ( 0.000000000000000000, 0.7540134720837716742, 0.6568589528324746407 ) ) ;
#15027 = LINE ( 'NONE', #1101, #16431 ) ;
#15028 = CARTESIAN_POINT ( 'NONE',  ( 38.00113996487114321, -17.91368208888609459, 72.53360434286904024 ) ) ;
#15029 = ORIENTED_EDGE ( 'NONE', *, *, #11831, .F. ) ;
#15030 = ORIENTED_EDGE ( 'NONE', *, *, #3276, .F. ) ;
#15031 = FACE_OUTER_BOUND ( 'NONE', #7664, .T. ) ;
#15032 = CARTESIAN_POINT ( 'NONE',  ( 39.75915168707250302, -0.7136820888860997414, 70.26145752964252722 ) ) ;
#15033 = CARTESIAN_POINT ( 'NONE',  ( 39.29254315202757653, -20.80384086642191832, 72.81632618279321889 ) ) ;
#15034 = CYLINDRICAL_SURFACE ( 'NONE', #6683, 1.499999999999999778 ) ;
#15035 = CARTESIAN_POINT ( 'NONE',  ( 39.64521430340304420, -2.813682088886101162, 69.45876917294177133 ) ) ;
#15036 = DIRECTION ( 'NONE',  ( 2.792262043613788535E-15, -0.8967398287344627850, -0.4425581086832399147 ) ) ;
#15037 = EDGE_LOOP ( 'NONE', ( #1994, #8663, #11718, #24638 ) ) ;
#15038 = CARTESIAN_POINT ( 'NONE',  ( 36.06606138205694378, 4.754708485422509234, 4.090082623941899698 ) ) ;
#15039 = CARTESIAN_POINT ( 'NONE',  ( 33.31606138205700773, -2.373793412309109563, 19.60611914621674146 ) ) ;
#15040 = CARTESIAN_POINT ( 'NONE',  ( 43.31606138205700773, -19.73594837544666802, 24.33996001444790025 ) ) ;
#15041 = CARTESIAN_POINT ( 'NONE',  ( 33.31606138205700773, -5.204193249396277032, 83.30501292736992980 ) ) ;
#15042 = LINE ( 'NONE', #20590, #22958 ) ;
#15043 = PRODUCT_DEFINITION_SHAPE ( 'NONE', 'NONE',  #8861 ) ;
#15044 = FACE_OUTER_BOUND ( 'NONE', #20682, .T. ) ;
#15045 = ORIENTED_EDGE ( 'NONE', *, *, #7893, .F. ) ;
#15046 = CARTESIAN_POINT ( 'NONE',  ( 33.31606138205700773, -4.357181138186123626, 83.30501292736992980 ) ) ;
#15047 = LINE ( 'NONE', #23029, #835 ) ;
#15048 = ORIENTED_EDGE ( 'NONE', *, *, #15465, .F. ) ;
#15049 = ORIENTED_EDGE ( 'NONE', *, *, #20204, .T. ) ;
#15050 = CARTESIAN_POINT ( 'NONE',  ( 37.61123632939164452, -15.70384086642191157, 69.02690120949091579 ) ) ;
#15051 = PLANE ( 'NONE',  #481 ) ;
#15052 = CARTESIAN_POINT ( 'NONE',  ( 39.95015449827720744, -20.61368208888610454, 70.79240656858105751 ) ) ;
#15053 = AXIS2_PLACEMENT_3D ( 'NONE', #6204, #4148, #12017 ) ;
#15054 = FILL_AREA_STYLE_COLOUR ( '', #3441 ) ;
#15055 = EDGE_LOOP ( 'NONE', ( #3482, #501, #20157, #14503 ) ) ;
#15056 = LINE ( 'NONE', #24451, #1016 ) ;
#15057 = DIRECTION ( 'NONE',  ( 2.792262043613788141E-15, -0.8967398287344626739, -0.4425581086832399147 ) ) ;
#15058 = CARTESIAN_POINT ( 'NONE',  ( 36.98690846071097837, -21.81368208888610738, 73.30173637941818754 ) ) ;
#15059 = ORIENTED_EDGE ( 'NONE', *, *, #8500, .T. ) ;
#15060 = EDGE_CURVE ( 'NONE', #21390, #14213, #16988, .T. ) ;
#15061 = CARTESIAN_POINT ( 'NONE',  ( 46.81606138205697221, -5.528433326023598049, -4.448224773462933435 ) ) ;
#15062 = CARTESIAN_POINT ( 'NONE',  ( 37.69796330110504101, 0.8863179111139003474, 69.66206559358664663 ) ) ;
#15063 = DIRECTION ( 'NONE',  ( 2.792262043613788535E-15, -0.8967398287344626739, -0.4425581086832399147 ) ) ;
#15064 = ADVANCED_FACE ( 'NONE', ( #3946 ), #3811, .T. ) ;
#15065 = CARTESIAN_POINT ( 'NONE',  ( 37.80618814713140097, -13.91368208888610702, 73.13360434286903455 ) ) ;
#15066 = EDGE_CURVE ( 'NONE', #6859, #1793, #1870, .T. ) ;
#15067 = ADVANCED_FACE ( 'NONE', ( #6136 ), #13996, .F. ) ;
#15068 = ADVANCED_FACE ( 'NONE', ( #16042 ), #571, .T. ) ;
#15069 = CARTESIAN_POINT ( 'NONE',  ( 33.40372220903689282, 3.256620197766214808, 6.241553153455755343 ) ) ;
#15070 = CARTESIAN_POINT ( 'NONE',  ( 33.31606138205700773, -21.39087554181787354, 28.82307548518891238 ) ) ;
#15071 = CARTESIAN_POINT ( 'NONE',  ( 39.31564783533279694, -17.30384086642191477, 70.72433947564853440 ) ) ;
#15072 = CARTESIAN_POINT ( 'NONE',  ( 39.98359781491296161, -8.413682088886105248, 71.86517103874048473 ) ) ;
#15073 = ORIENTED_EDGE ( 'NONE', *, *, #20775, .T. ) ;
#15074 = CARTESIAN_POINT ( 'NONE',  ( 44.81606138205700063, -24.55876147765401996, 67.80501292737008612 ) ) ;
#15075 = EDGE_CURVE ( 'NONE', #19555, #4227, #10640, .T. ) ;
#15076 = ORIENTED_EDGE ( 'NONE', *, *, #7059, .F. ) ;
#15077 = EDGE_CURVE ( 'NONE', #22818, #19683, #6392, .T. ) ;
#15078 = VERTEX_POINT ( 'NONE', #18122 ) ;
#15079 = CARTESIAN_POINT ( 'NONE',  ( 39.95015449827720744, -3.003840866421910505, 71.96809898377888715 ) ) ;
#15080 = DIRECTION ( 'NONE',  ( 0.000000000000000000, 0.7540134720837676774, 0.6568589528324791926 ) ) ;
#15081 = CARTESIAN_POINT ( 'NONE',  ( 37.69796330110504101, 0.8863179111139003474, 69.66206559358664663 ) ) ;
#15082 = ORIENTED_EDGE ( 'NONE', *, *, #15615, .F. ) ;
#15083 = CARTESIAN_POINT ( 'NONE',  ( 40.52078840805428683, -6.613682088886105426, 70.60699637195608602 ) ) ;
#15084 = ORIENTED_EDGE ( 'NONE', *, *, #20979, .F. ) ;
#15085 = FACE_OUTER_BOUND ( 'NONE', #11939, .T. ) ;
#15086 = CARTESIAN_POINT ( 'NONE',  ( 37.69225076346193504, -5.803840866421911215, 70.42958956619168021 ) ) ;
#15087 = AXIS2_PLACEMENT_3D ( 'NONE', #15264, #23631, #15773 ) ;
#15088 = CIRCLE ( 'NONE', #17584, 0.9999999999999937828 ) ;
#15089 = DIRECTION ( 'NONE',  ( -0.000000000000000000, -3.469446951953613400E-15, -1.000000000000000000 ) ) ;
#15090 = ORIENTED_EDGE ( 'NONE', *, *, #2786, .T. ) ;
#15091 = LINE ( 'NONE', #22945, #10089 ) ;
#15092 = LINE ( 'NONE', #20513, #23970 ) ;
#15093 = CARTESIAN_POINT ( 'NONE',  ( 40.52078840805429394, -19.00384086642191406, 72.15350918040381600 ) ) ;
#15094 = CARTESIAN_POINT ( 'NONE',  ( 37.09113907096683960, -21.80759215409126739, 75.30824661320679070 ) ) ;
#15095 = CARTESIAN_POINT ( 'NONE',  ( 38.93415946300897446, -18.11368208888611164, 73.09843995877329803 ) ) ;
#15096 = CARTESIAN_POINT ( 'NONE',  ( 33.31606138205700773, -26.06829118875199924, 75.30501292736998664 ) ) ;
#15097 = DIRECTION ( 'NONE',  ( -1.000000000000000000, 6.018531076210110289E-31, 1.734723475976804876E-16 ) ) ;
#15098 = EDGE_CURVE ( 'NONE', #13035, #15148, #14500, .T. ) ;
#15099 = ORIENTED_EDGE ( 'NONE', *, *, #20191, .F. ) ;
#15100 = PLANE ( 'NONE',  #24772 ) ;
#15101 = DIRECTION ( 'NONE',  ( -1.000000000000000000, 0.000000000000000000, 0.000000000000000000 ) ) ;
#15102 = CARTESIAN_POINT ( 'NONE',  ( 39.29254315202757653, -8.803840866421912992, 72.81632618279323310 ) ) ;
#15103 = CIRCLE ( 'NONE', #19624, 1.000000000000000888 ) ;
#15104 = CARTESIAN_POINT ( 'NONE',  ( 33.09672011123848279, 3.247905043202620856, 6.142517800649935467 ) ) ;
#15105 = CARTESIAN_POINT ( 'NONE',  ( 36.68196826583682935, -27.61368208888610809, 71.96809898377887293 ) ) ;
#15106 = VECTOR ( 'NONE', #20651, 1000.000000000000000 ) ;
#15107 = VECTOR ( 'NONE', #17112, 1000.000000000000000 ) ;
#15108 = CARTESIAN_POINT ( 'NONE',  ( 31.81606138205700418, 18.19123852234599426, 73.05501292736995822 ) ) ;
#15109 = EDGE_CURVE ( 'NONE', #9497, #19656, #10379, .T. ) ;
#15110 = CARTESIAN_POINT ( 'NONE',  ( 39.95015449827720744, -25.00384086642191406, 71.96809898377885872 ) ) ;
#15111 = CARTESIAN_POINT ( 'NONE',  ( 36.31606138205700063, -6.942307388142325841, 83.16359031225202614 ) ) ;
#15112 = CARTESIAN_POINT ( 'NONE',  ( 36.49096545463212493, -17.51368208888610667, 71.43714994484034264 ) ) ;
#15113 = ORIENTED_EDGE ( 'NONE', *, *, #18953, .T. ) ;
#15114 = CARTESIAN_POINT ( 'NONE',  ( 35.86008812008917346, -25.51368208888610667, 71.43714994484032843 ) ) ;
#15115 = ORIENTED_EDGE ( 'NONE', *, *, #18942, .F. ) ;
#15116 = DIRECTION ( 'NONE',  ( -1.000000000000000000, -1.734723475976804876E-16, 1.734723475976814737E-16 ) ) ;
#15117 = DIRECTION ( 'NONE',  ( -1.000000000000000000, 0.000000000000000000, 0.000000000000000000 ) ) ;
#15118 = CARTESIAN_POINT ( 'NONE',  ( 39.24876120206128860, 1.286317911113898260, 70.63227792289248441 ) ) ;
#15119 = EDGE_LOOP ( 'NONE', ( #25343, #11143, #4709, #21389 ) ) ;
#15120 = EDGE_CURVE ( 'NONE', #3155, #8442, #444, .T. ) ;
#15121 = ORIENTED_EDGE ( 'NONE', *, *, #14465, .T. ) ;
#15122 = FACE_OUTER_BOUND ( 'NONE', #5599, .T. ) ;
#15123 = CARTESIAN_POINT ( 'NONE',  ( 33.31606138205700773, -20.88462213363798270, 44.49284693533410717 ) ) ;
#15124 = ORIENTED_EDGE ( 'NONE', *, *, #3161, .T. ) ;
#15125 = DIRECTION ( 'NONE',  ( 0.000000000000000000, 1.000000000000000000, -2.921639538487253867E-15 ) ) ;
#15126 = CARTESIAN_POINT ( 'NONE',  ( 39.38009889167648936, -5.403840866421906419, 70.00779233799264034 ) ) ;
#15127 = EDGE_CURVE ( 'NONE', #1199, #14256, #12327, .T. ) ;
#15128 = VECTOR ( 'NONE', #20937, 1000.000000000000000 ) ;
#15129 = AXIS2_PLACEMENT_3D ( 'NONE', #17499, #15166, #1750 ) ;
#15130 = DIRECTION ( 'NONE',  ( -2.365532012695645428E-15, 1.000000000000000000, 0.000000000000000000 ) ) ;
#15131 = PLANE ( 'NONE',  #19207 ) ;
#15132 = ORIENTED_EDGE ( 'NONE', *, *, #3125, .F. ) ;
#15133 = ORIENTED_EDGE ( 'NONE', *, *, #4566, .T. ) ;
#15134 = CARTESIAN_POINT ( 'NONE',  ( 32.31606138205700063, -20.93319939328399926, 43.78741072286599945 ) ) ;
#15135 = CARTESIAN_POINT ( 'NONE',  ( 37.69796330110504101, 0.8863179111139005695, 69.66206559358666084 ) ) ;
#15136 = CARTESIAN_POINT ( 'NONE',  ( 37.25202387243754032, -26.40384086642191619, 72.75271321436730432 ) ) ;
#15137 = SURFACE_STYLE_FILL_AREA ( #11544 ) ;
#15138 = PLANE ( 'NONE',  #21103 ) ;
#15139 = ORIENTED_EDGE ( 'NONE', *, *, #18714, .F. ) ;
#15140 = DIRECTION ( 'NONE',  ( 1.327674326049719602E-15, -0.4425581086832399147, 0.8967398287344627850 ) ) ;
#15141 = AXIS2_PLACEMENT_3D ( 'NONE', #24040, #14265, #23788 ) ;
#15142 = DIRECTION ( 'NONE',  ( -1.000000000000000000, 0.000000000000000000, 0.000000000000000000 ) ) ;
#15143 = DIRECTION ( 'NONE',  ( 2.690219486203388234E-15, -0.8967398287344627850, -0.4425581086832399147 ) ) ;
#15144 = EDGE_LOOP ( 'NONE', ( #9073, #169, #7601, #2382 ) ) ;
#15145 = VECTOR ( 'NONE', #18720, 1000.000000000000000 ) ;
#15146 = CIRCLE ( 'NONE', #9389, 1.000000000000000000 ) ;
#15147 = CARTESIAN_POINT ( 'NONE',  ( 30.81606138205700418, -26.74044063519535186, 82.55501292737007191 ) ) ;
#15148 = VERTEX_POINT ( 'NONE', #14494 ) ;
#15149 = ORIENTED_EDGE ( 'NONE', *, *, #6875, .F. ) ;
#15151 = EDGE_CURVE ( 'NONE', #15078, #1612, #6286, .T. ) ;
#15150 = DIRECTION ( 'NONE',  ( 3.028377322213060447E-31, 1.000000000000000000, -2.999999999999999839E-15 ) ) ;
#15152 = CARTESIAN_POINT ( 'NONE',  ( 40.31606138205701484, -20.02093502212014897, 26.61211107664843212 ) ) ;
#15153 = EDGE_CURVE ( 'NONE', #19678, #12694, #20038, .T. ) ;
#15154 = CARTESIAN_POINT ( 'NONE',  ( 37.31647492878122563, -15.31368208888610205, 70.72433947564853440 ) ) ;
#15155 = EDGE_LOOP ( 'NONE', ( #23193, #9804, #11434, #8378 ) ) ;
#15156 = EDGE_CURVE ( 'NONE', #24251, #15261, #2381, .T. ) ;
#15157 = VERTEX_POINT ( 'NONE', #14619 ) ;
#15158 = CARTESIAN_POINT ( 'NONE',  ( 36.81465384343994884, 41.67000142393845152, 79.52109337493035923 ) ) ;
#15159 = DIRECTION ( 'NONE',  ( -1.000000000000000000, -2.954840238787252245E-15, -9.150562545582958565E-17 ) ) ;
#15160 = CARTESIAN_POINT ( 'NONE',  ( 39.95015449827720744, -25.00384086642191406, 71.96809898377885872 ) ) ;
#15161 = CARTESIAN_POINT ( 'NONE',  ( 42.99362139871320210, 2.839053109165292632, 6.102835131782519795 ) ) ;
#15162 = ORIENTED_EDGE ( 'NONE', *, *, #15397, .F. ) ;
#15163 = VECTOR ( 'NONE', #13600, 1000.000000000000000 ) ;
#15164 = DIRECTION ( 'NONE',  ( 0.000000000000000000, -0.7516416929448760387, -0.6595716529892418079 ) ) ;
#15165 = ADVANCED_FACE ( 'NONE', ( #10256 ), #18366, .T. ) ;
#15166 = DIRECTION ( 'NONE',  ( 1.425933913527082566E-16, -0.9038432971286278761, -0.4278636397681519488 ) ) ;
#15167 = CARTESIAN_POINT ( 'NONE',  ( 39.31606138205700063, 43.19123852234595518, 61.30501292736988006 ) ) ;
#15168 = VECTOR ( 'NONE', #17015, 1000.000000000000000 ) ;
#15169 = DIRECTION ( 'NONE',  ( 0.000000000000000000, 1.163336342344340343E-15, -1.000000000000000000 ) ) ;
#15170 = DIRECTION ( 'NONE',  ( 0.000000000000000000, -0.5706330172266913525, 0.8212051873014213355 ) ) ;
#15171 = AXIS2_PLACEMENT_3D ( 'NONE', #24894, #7273, #15125 ) ;
#15172 = CARTESIAN_POINT ( 'NONE',  ( 31.81606138205700418, -34.55876147765401640, 70.30501292737011454 ) ) ;
#15173 = CARTESIAN_POINT ( 'NONE',  ( 45.81606138205697221, -3.863943790789048816, -7.177613496534156035 ) ) ;
#15174 = CARTESIAN_POINT ( 'NONE',  ( 39.81606138205699352, 6.191238522346988127, 65.30501292736998664 ) ) ;
#15175 = ORIENTED_EDGE ( 'NONE', *, *, #3655, .F. ) ;
#15176 = ORIENTED_EDGE ( 'NONE', *, *, #4836, .F. ) ;
#15177 = CARTESIAN_POINT ( 'NONE',  ( 40.26954217208372455, -12.90384086642192152, 72.86986841596734621 ) ) ;
#15178 = AXIS2_PLACEMENT_3D ( 'NONE', #18104, #15648, #19769 ) ;
#15179 = PLANE ( 'NONE',  #20656 ) ;
#15180 = CARTESIAN_POINT ( 'NONE',  ( 39.95015449827720744, -14.61368208888610454, 70.79240656858105751 ) ) ;
#15181 = ORIENTED_EDGE ( 'NONE', *, *, #24809, .T. ) ;
#15182 = CARTESIAN_POINT ( 'NONE',  ( 29.71606138205697789, -6.210967385200577340, -3.065230171572522977 ) ) ;
#15183 = DIRECTION ( 'NONE',  ( 0.000000000000000000, -1.000000000000000000, 2.999999999999999839E-15 ) ) ;
#15184 = CARTESIAN_POINT ( 'NONE',  ( 37.61123632939165873, -19.91368208888610880, 73.73360434286898624 ) ) ;
#15185 = VERTEX_POINT ( 'NONE', #20169 ) ;
#15186 = VECTOR ( 'NONE', #2296, 1000.000000000000000 ) ;
#15187 = PRESENTATION_STYLE_ASSIGNMENT (( #24842 ) ) ;
#15188 = DIRECTION ( 'NONE',  ( 1.000000000000000000, 2.805550545906362824E-15, -9.596449257708899394E-17 ) ) ;
#15189 = DIRECTION ( 'NONE',  ( 1.836970198721029688E-16, 2.999999999999999839E-15, 1.000000000000000000 ) ) ;
#15190 = EDGE_CURVE ( 'NONE', #12627, #546, #16288, .T. ) ;
#15191 = VECTOR ( 'NONE', #5290, 1000.000000000000000 ) ;
#15192 = CARTESIAN_POINT ( 'NONE',  ( 30.81606138205697576, -3.984974717493129592, -3.847356352999882656 ) ) ;
#15193 = CARTESIAN_POINT ( 'NONE',  ( 36.80507328770344344, -5.887228176602778973, 83.28319385500074645 ) ) ;
#15194 = CIRCLE ( 'NONE', #4110, 0.7500000000000027756 ) ;
#15195 = CARTESIAN_POINT ( 'NONE',  ( 38.73920764526923932, -19.50384086642191406, 70.26206559358661252 ) ) ;
#15196 = CARTESIAN_POINT ( 'NONE',  ( 37.69225076346193504, -27.81368208888610383, 72.33091598616823603 ) ) ;
#15197 = ORIENTED_EDGE ( 'NONE', *, *, #4054, .T. ) ;
#15198 = VECTOR ( 'NONE', #17566, 1000.000000000000227 ) ;
#15199 = LINE ( 'NONE', #25230, #3662 ) ;
#15200 = DIRECTION ( 'NONE',  ( 0.000000000000000000, 0.6568589528324746407, -0.7540134720837717852 ) ) ;
#15201 = ORIENTED_EDGE ( 'NONE', *, *, #14232, .F. ) ;
#15202 = ORIENTED_EDGE ( 'NONE', *, *, #11159, .F. ) ;
#15203 = VECTOR ( 'NONE', #3159, 1000.000000000000000 ) ;
#15204 = CARTESIAN_POINT ( 'NONE',  ( 39.82603832034400426, -1.303840866421906997, 70.35351908239857721 ) ) ;
#15205 = EDGE_CURVE ( 'NONE', #23679, #24313, #10805, .T. ) ;
#15206 = EDGE_CURVE ( 'NONE', #8670, #23160, #4588, .T. ) ;
#15207 = CARTESIAN_POINT ( 'NONE',  ( 38.93415946300897446, -2.113682088886109423, 73.09843995877331224 ) ) ;
#15208 = CARTESIAN_POINT ( 'NONE',  ( 40.33642880535524000, -8.313682088886110932, 72.77780686321128201 ) ) ;
#15209 = VECTOR ( 'NONE', #13932, 1000.000000000000000 ) ;
#15210 = ORIENTED_EDGE ( 'NONE', *, *, #2154, .T. ) ;
#15211 = DIRECTION ( 'NONE',  ( 0.000000000000000000, 1.000000000000000000, -2.999999999999999839E-15 ) ) ;
#15212 = CARTESIAN_POINT ( 'NONE',  ( 38.00113996487112189, -7.703840866421914235, 70.22690120949091863 ) ) ;
#15213 = EDGE_CURVE ( 'NONE', #13483, #16994, #10512, .T. ) ;
#15214 = LINE ( 'NONE', #13299, #20460 ) ;
#15215 = EDGE_LOOP ( 'NONE', ( #8702, #23536, #6133, #10003, #17978, #13407, #16509, #12709, #3107, #7025, #21332, #3068, #12009 ) ) ;
#15216 = CARTESIAN_POINT ( 'NONE',  ( 41.31606138205700063, 14.21032488318011211, 61.14033482768515881 ) ) ;
#15217 = DIRECTION ( 'NONE',  ( -1.000000000000000000, 5.204170427930413997E-31, 1.734723475976804876E-16 ) ) ;
#15218 = CARTESIAN_POINT ( 'NONE',  ( 40.77203464402485622, -7.103840866421913702, 71.43714994484034264 ) ) ;
#15219 = CARTESIAN_POINT ( 'NONE',  ( 37.66883992158368955, -22.12333347212302925, 75.80539787555638043 ) ) ;
#15220 = CARTESIAN_POINT ( 'NONE',  ( 37.25202387243752611, -11.21368208888610241, 70.00779233799262613 ) ) ;
#15221 = CARTESIAN_POINT ( 'NONE',  ( 44.06606138205700063, 40.39281886181299797, 84.30501292736984453 ) ) ;
#15222 = CIRCLE ( 'NONE', #16053, 1.499999999999999778 ) ;
#15223 = EDGE_CURVE ( 'NONE', #22382, #16518, #20416, .T. ) ;
#15224 = CARTESIAN_POINT ( 'NONE',  ( 33.31606138205700773, -16.48551471403133206, 77.11349248448009064 ) ) ;
#15225 = AXIS2_PLACEMENT_3D ( 'NONE', #7934, #23877, #300 ) ;
#15226 = ORIENTED_EDGE ( 'NONE', *, *, #5176, .T. ) ;
#15227 = CARTESIAN_POINT ( 'NONE',  ( 39.81746892067405952, 41.90149715599300606, 79.87823623207322044 ) ) ;
#15228 = AXIS2_PLACEMENT_3D ( 'NONE', #6697, #6202, #18430 ) ;
#15229 = CARTESIAN_POINT ( 'NONE',  ( 38.37017380507018771, -9.603840866421908373, 69.64448340153879258 ) ) ;
#15230 = SHAPE_DEFINITION_REPRESENTATION ( #17966, #15514 ) ;
#15231 = CARTESIAN_POINT ( 'NONE',  ( 32.85323118609060344, 3.754743573466622575, 6.231177976620378978 ) ) ;
#15232 = CARTESIAN_POINT ( 'NONE',  ( 38.82593461698262871, -24.91368208888610170, 69.62690120949091011 ) ) ;
#15233 = APPLICATION_CONTEXT ( 'automotive_design' ) ;
#15234 = DIRECTION ( 'NONE',  ( 0.000000000000000000, 0.5706330172266915746, -0.8212051873014213355 ) ) ;
#15235 = B_SPLINE_CURVE_WITH_KNOTS ( 'NONE', 3,
 ( #14338, #22193, #4795, #14223 ),
 .UNSPECIFIED., .F., .F.,
 ( 4, 4 ),
 ( 0.000000000000000000, 1.000000000000000000 ),
 .UNSPECIFIED. ) ;
#15236 = CARTESIAN_POINT ( 'NONE',  ( 39.95015449827720744, -17.00384086642191406, 71.96809898377887293 ) ) ;
#15237 = CARTESIAN_POINT ( 'NONE',  ( 36.36697178183959522, -6.614802349578126517, 82.70773085854241913 ) ) ;
#15238 = EDGE_CURVE ( 'NONE', #4719, #9093, #24394, .T. ) ;
#15239 = AXIS2_PLACEMENT_3D ( 'NONE', #4336, #4457, #20544 ) ;
#15240 = CARTESIAN_POINT ( 'NONE',  ( 40.14115730948191185, -18.51368208888610667, 71.32335560751960202 ) ) ;
#15241 = EDGE_LOOP ( 'NONE', ( #19448, #14523 ) ) ;
#15242 = CARTESIAN_POINT ( 'NONE',  ( 38.37017380507018771, 0.3961591335780896284, 69.04448340153882668 ) ) ;
#15243 = ORIENTED_EDGE ( 'NONE', *, *, #1686, .T. ) ;
#15244 = CARTESIAN_POINT ( 'NONE',  ( 43.06606138205700063, 43.19123852234599070, 73.55501292736987295 ) ) ;
#15245 = DIRECTION ( 'NONE',  ( -6.489379976170840313E-31, 1.000000000000000000, -3.491481338843135327E-15 ) ) ;
#15246 = VECTOR ( 'NONE', #24559, 1000.000000000000000 ) ;
#15247 = CARTESIAN_POINT ( 'NONE',  ( 38.00113996487112189, -23.70384086642191335, 70.22690120949089021 ) ) ;
#15248 = ADVANCED_FACE ( 'NONE', ( #8196, #8710, #16542, #12073 ), #9226, .F. ) ;
#15249 = ADVANCED_FACE ( 'NONE', ( #3010 ), #22980, .F. ) ;
#15250 = ORIENTED_EDGE ( 'NONE', *, *, #6905, .F. ) ;
#15251 = ORIENTED_EDGE ( 'NONE', *, *, #10233, .F. ) ;
#15252 = LINE ( 'NONE', #3141, #19114 ) ;
#15253 = FACE_OUTER_BOUND ( 'NONE', #827, .T. ) ;
#15254 = ORIENTED_EDGE ( 'NONE', *, *, #19815, .T. ) ;
#15255 = SURFACE_STYLE_USAGE ( .BOTH. , #25020 ) ;
#15256 = CARTESIAN_POINT ( 'NONE',  ( 40.77203464402485622, -29.10384086642191193, 71.43714994484031422 ) ) ;
#15257 = CARTESIAN_POINT ( 'NONE',  ( 43.47464771180118248, 3.634064700962194028, 6.274728512395983948 ) ) ;
#15258 = EDGE_CURVE ( 'NONE', #4551, #11492, #12955, .T. ) ;
#15259 = DIRECTION ( 'NONE',  ( 1.000000000000000000, 0.000000000000000000, 0.000000000000000000 ) ) ;
#15260 = ORIENTED_EDGE ( 'NONE', *, *, #20449, .T. ) ;
#15261 = VERTEX_POINT ( 'NONE', #24768 ) ;
#15262 = CARTESIAN_POINT ( 'NONE',  ( 40.81606138205700773, 37.44123852234599781, 74.30501292736988717 ) ) ;
#15263 = AXIS2_PLACEMENT_3D ( 'NONE', #12763, #6947, #24704 ) ;
#15264 = CARTESIAN_POINT ( 'NONE',  ( 44.81606138205700063, 35.95440708241085304, 62.30501292736990138 ) ) ;
#15265 = LINE ( 'NONE', #24904, #21716 ) ;
#15266 = CYLINDRICAL_SURFACE ( 'NONE', #4637, 0.4999999999999982792 ) ;
#15267 = AXIS2_PLACEMENT_3D ( 'NONE', #23123, #25302, #21456 ) ;
#15268 = VERTEX_POINT ( 'NONE', #7150 ) ;
#15269 = CYLINDRICAL_SURFACE ( 'NONE', #8593, 0.7500000000000006661 ) ;
#15270 = ADVANCED_FACE ( 'NONE', ( #951 ), #5092, .F. ) ;
#15271 = DIRECTION ( 'NONE',  ( -1.734723475976804876E-16, -3.491481338843135327E-15, -1.000000000000000000 ) ) ;
#15272 = LINE ( 'NONE', #9622, #15504 ) ;
#15273 = SURFACE_STYLE_USAGE ( .BOTH. , #18633 ) ;
#15274 = ORIENTED_EDGE ( 'NONE', *, *, #4532, .F. ) ;
#15275 = CARTESIAN_POINT ( 'NONE',  ( 44.81606138205700063, -21.15876147765410309, 66.30501292737000085 ) ) ;
#15276 = VERTEX_POINT ( 'NONE', #18608 ) ;
#15277 = EDGE_LOOP ( 'NONE', ( #19882, #20707, #15723, #5836 ) ) ;
#15278 = CARTESIAN_POINT ( 'NONE',  ( 33.31606138205700773, 4.124002793203064066, 6.312068993173404863 ) ) ;
#15279 = CARTESIAN_POINT ( 'NONE',  ( 38.73920764526925353, -14.11368208888610098, 72.49843995877330372 ) ) ;
#15280 = CARTESIAN_POINT ( 'NONE',  ( 38.73920764526925353, -14.11368208888610098, 72.49843995877330372 ) ) ;
#15281 = ORIENTED_EDGE ( 'NONE', *, *, #18856, .F. ) ;
#15282 = ORIENTED_EDGE ( 'NONE', *, *, #10497, .T. ) ;
#15283 = PLANE ( 'NONE',  #7103 ) ;
#15284 = CARTESIAN_POINT ( 'NONE',  ( 39.38009889167650357, 1.786317911113891821, 72.75271321436734695 ) ) ;
#15285 = CARTESIAN_POINT ( 'NONE',  ( 36.64852494920107517, -24.20384086642190979, 71.86517103874047052 ) ) ;
#15286 = DIRECTION ( 'NONE',  ( 1.327674326049719602E-15, -0.4425581086832399147, 0.8967398287344627850 ) ) ;
#15287 = AXIS2_PLACEMENT_3D ( 'NONE', #8651, #6453, #12015 ) ;
#15288 = CARTESIAN_POINT ( 'NONE',  ( 38.73920764526925353, -20.11368208888610098, 72.49843995877330372 ) ) ;
#15289 = ORIENTED_EDGE ( 'NONE', *, *, #10193, .T. ) ;
#15290 = CARTESIAN_POINT ( 'NONE',  ( 3.816061382056972207, -5.823060841851324554, -8.896754523299009065 ) ) ;
#15291 = PLANE ( 'NONE',  #4005 ) ;
#15292 = EDGE_CURVE ( 'NONE', #5806, #21711, #8841, .T. ) ;
#15293 = DIRECTION ( 'NONE',  ( -1.000000000000000000, 0.000000000000000000, 0.000000000000000000 ) ) ;
#15294 = ADVANCED_FACE ( 'NONE', ( #15001 ), #10768, .T. ) ;
#15295 = CARTESIAN_POINT ( 'NONE',  ( 39.64148445914975127, -5.677091398499680253, 82.79421705341921722 ) ) ;
#15296 = LINE ( 'NONE', #11710, #23373 ) ;
#15297 = ADVANCED_FACE ( 'NONE', ( #24892 ), #11146, .F. ) ;
#15298 = VECTOR ( 'NONE', #23898, 1000.000000000000000 ) ;
#15299 = CIRCLE ( 'NONE', #17365, 0.7106531558045068309 ) ;
#15300 = LINE ( 'NONE', #13762, #8619 ) ;
#15301 = ORIENTED_EDGE ( 'NONE', *, *, #10516, .T. ) ;
#15302 = CARTESIAN_POINT ( 'NONE',  ( 43.81606138205700063, -27.66931681479738003, 59.51410614687260647 ) ) ;
#15303 = AXIS2_PLACEMENT_3D ( 'NONE', #5026, #14942, #24578 ) ;
#15304 = CARTESIAN_POINT ( 'NONE',  ( 45.81606138205695089, -5.823060841851306790, -8.896754523299028605 ) ) ;
#15305 = EDGE_LOOP ( 'NONE', ( #906, #22090, #5993, #22915, #22543 ) ) ;
#15306 = ORIENTED_EDGE ( 'NONE', *, *, #10967, .F. ) ;
#15307 = CARTESIAN_POINT ( 'NONE',  ( 38.37017380507018771, -11.60384086642191015, 69.04448340153881247 ) ) ;
#15308 = ADVANCED_FACE ( 'NONE', ( #4959 ), #7271, .T. ) ;
#15309 = CARTESIAN_POINT ( 'NONE',  ( 42.82259846190797248, 3.224889648804766473, 6.370942050318627814 ) ) ;
#15310 = CARTESIAN_POINT ( 'NONE',  ( 38.82593461698262871, -12.91368208888610347, 69.62690120949091011 ) ) ;
#15311 = SHAPE_REPRESENTATION_RELATIONSHIP ( 'NONE' , 'NONE' ,  #14684, #15967 ) ;
#15312 = ORIENTED_EDGE ( 'NONE', *, *, #7450, .F. ) ;
#15313 = CARTESIAN_POINT ( 'NONE',  ( 30.81606138205700418, -34.55876147765410167, 66.30501292737000085 ) ) ;
#15314 = FACE_OUTER_BOUND ( 'NONE', #7882, .T. ) ;
#15315 = CARTESIAN_POINT ( 'NONE',  ( 39.02088643472237095, -22.91368208888609814, 69.02690120949091579 ) ) ;
#15316 = ORIENTED_EDGE ( 'NONE', *, *, #4831, .T. ) ;
#15317 = VECTOR ( 'NONE', #6430, 1000.000000000000000 ) ;
#15318 = CARTESIAN_POINT ( 'NONE',  ( 43.81606138205700063, 41.44123852234595518, 61.30501292736988006 ) ) ;
#15319 = CYLINDRICAL_SURFACE ( 'NONE', #7381, 4.000000000000000000 ) ;
#15320 = PLANE ( 'NONE',  #10396 ) ;
#15321 = AXIS2_PLACEMENT_3D ( 'NONE', #23771, #23383, #7818 ) ;
#15322 = DIRECTION ( 'NONE',  ( 1.734723475976804876E-16, -1.000000000000000000, -3.009265538105065326E-32 ) ) ;
#15323 = CIRCLE ( 'NONE', #5050, 1.000000000000000888 ) ;
#15324 = CIRCLE ( 'NONE', #14103, 10.00000000000000000 ) ;
#15325 = LINE ( 'NONE', #9543, #5513 ) ;
#15326 = CARTESIAN_POINT ( 'NONE',  ( 38.63098279924290068, -14.70384086642191157, 72.53360434286904024 ) ) ;
#15327 = CARTESIAN_POINT ( 'NONE',  ( 38.93415946300897446, 1.886317911113891244, 73.09843995877332645 ) ) ;
#15328 = ORIENTED_EDGE ( 'NONE', *, *, #12367, .F. ) ;
#15329 = DIRECTION ( 'NONE',  ( 1.117439894383781939E-44, -1.000000000000000000, 2.999999999999993528E-15 ) ) ;
#15330 = AXIS2_PLACEMENT_3D ( 'NONE', #4499, #20950, #16697 ) ;
#15331 = LINE ( 'NONE', #23567, #8660 ) ;
#15332 = ORIENTED_EDGE ( 'NONE', *, *, #19977, .T. ) ;
#15333 = ORIENTED_EDGE ( 'NONE', *, *, #3578, .F. ) ;
#15334 = AXIS2_PLACEMENT_3D ( 'NONE', #14010, #707, #21863 ) ;
#15335 = CARTESIAN_POINT ( 'NONE',  ( 37.33957961208645315, 0.1961591335780908663, 69.94417936956673998 ) ) ;
#15336 = EDGE_CURVE ( 'NONE', #1959, #5217, #12828, .T. ) ;
#15337 = VECTOR ( 'NONE', #24478, 1000.000000000000000 ) ;
#15338 = CARTESIAN_POINT ( 'NONE',  ( 38.37017380507020192, 1.986317911113890444, 73.11602215082119471 ) ) ;
#15339 = CARTESIAN_POINT ( 'NONE',  ( 37.50301148336529167, -1.113682088886101207, 69.06206559358666652 ) ) ;
#15340 = ORIENTED_EDGE ( 'NONE', *, *, #16478, .T. ) ;
#15341 = DIRECTION ( 'NONE',  ( 1.836970198721029688E-16, 2.999999999999999839E-15, 1.000000000000000000 ) ) ;
#15342 = CARTESIAN_POINT ( 'NONE',  ( 37.69225076346193504, -7.803840866421912104, 70.42958956619168021 ) ) ;
#15343 = DIRECTION ( 'NONE',  ( 0.000000000000000000, -0.8967398287344626739, -0.4425581086832399147 ) ) ;
#15344 = ORIENTED_EDGE ( 'NONE', *, *, #4047, .F. ) ;
#15345 = CARTESIAN_POINT ( 'NONE',  ( 43.81606138205700063, -33.70281195181703993, 69.07320514641659770 ) ) ;
#15346 = CYLINDRICAL_SURFACE ( 'NONE', #19473, 1.250000000000000888 ) ;
#15347 = CARTESIAN_POINT ( 'NONE',  ( 40.26954217208372455, -12.90384086642192152, 72.86986841596734621 ) ) ;
#15348 = DIRECTION ( 'NONE',  ( -1.000000000000000000, 1.809068767804384992E-15, 0.000000000000000000 ) ) ;
#15349 = CARTESIAN_POINT ( 'NONE',  ( 38.31606138205700773, -22.27515649656512053, 29.48506754039017963 ) ) ;
#15350 = CARTESIAN_POINT ( 'NONE',  ( 38.93415946300897446, -14.11368208888610631, 73.09843995877329803 ) ) ;
#15351 = FACE_OUTER_BOUND ( 'NONE', #7429, .T. ) ;
#15352 = CARTESIAN_POINT ( 'NONE',  ( 47.81606138205695800, 1.394403967322872306, -2.658592958638780424 ) ) ;
#15353 = AXIS2_PLACEMENT_3D ( 'NONE', #20525, #4940, #24490 ) ;
#15354 = CARTESIAN_POINT ( 'NONE',  ( 33.81606138205700063, 22.19123852234701388, 73.80501292736992980 ) ) ;
#15355 = AXIS2_PLACEMENT_3D ( 'NONE', #19592, #1933, #9818 ) ;
#15356 = CARTESIAN_POINT ( 'NONE',  ( 36.49096545463212493, -10.10384086642191193, 71.32335560751963044 ) ) ;
#15357 = APPLICATION_PROTOCOL_DEFINITION ( 'draft international standard', 'automotive_design', 1998, #16705 ) ;
#15358 = CARTESIAN_POINT ( 'NONE',  ( 33.56815104093937663, 3.421967759159691536, 6.351335392992072393 ) ) ;
#15359 = CARTESIAN_POINT ( 'NONE',  ( 39.95015449827720744, -16.61368208888610454, 70.79240656858105751 ) ) ;
#15360 = CARTESIAN_POINT ( 'NONE',  ( 43.06606138205700063, 42.19123852234599781, 74.30501292736987295 ) ) ;
#15361 = VECTOR ( 'NONE', #5225, 1000.000000000000000 ) ;
#15362 = CARTESIAN_POINT ( 'NONE',  ( 37.80618814713138676, -15.70384086642191157, 69.62690120949091011 ) ) ;
#15363 = CARTESIAN_POINT ( 'NONE',  ( 36.99159426505191561, -5.699776791028273948, 83.29373111488995107 ) ) ;
#15364 =( GEOMETRIC_REPRESENTATION_CONTEXT ( 3 ) GLOBAL_UNCERTAINTY_ASSIGNED_CONTEXT ( ( #23943 ) ) GLOBAL_UNIT_ASSIGNED_CONTEXT ( ( #3543, #7037, #12978 ) ) REPRESENTATION_CONTEXT ( 'NONE', 'WORKASPACE' ) );
#15365 = EDGE_CURVE ( 'NONE', #12687, #16840, #11013, .T. ) ;
#15366 = CARTESIAN_POINT ( 'NONE',  ( 37.33957961208646736, -15.81368208888610916, 72.81632618279321889 ) ) ;
#15367 = ORIENTED_EDGE ( 'NONE', *, *, #23266, .F. ) ;
#15368 = CARTESIAN_POINT ( 'NONE',  ( 36.36258059203031934, -21.71368208888610596, 72.86986841596736042 ) ) ;
#15369 = VERTEX_POINT ( 'NONE', #21059 ) ;
#15370 = DIRECTION ( 'NONE',  ( 2.011972697750610993E-15, -0.6595716529892349245, 0.7516416929448819229 ) ) ;
#15371 = AXIS2_PLACEMENT_3D ( 'NONE', #355, #13783, #9924 ) ;
#15372 = CYLINDRICAL_SURFACE ( 'NONE', #10839, 1.000000000000000888 ) ;
#15373 = CARTESIAN_POINT ( 'NONE',  ( 39.37952058850012804, -23.00384086642191050, 71.78268878715390144 ) ) ;
#15374 = ORIENTED_EDGE ( 'NONE', *, *, #17933, .F. ) ;
#15375 = ORIENTED_EDGE ( 'NONE', *, *, #14632, .T. ) ;
#15376 = CARTESIAN_POINT ( 'NONE',  ( 39.81606138205700063, -3.742417511052531509, 58.76316301854844681 ) ) ;
#15377 = AXIS2_PLACEMENT_3D ( 'NONE', #16292, #24022, #2883 ) ;
#15378 = LINE ( 'NONE', #1961, #16563 ) ;
#15379 = EDGE_LOOP ( 'NONE', ( #19646, #24391, #1084, #16945 ) ) ;
#15380 = CARTESIAN_POINT ( 'NONE',  ( 30.81606138205700418, 40.39281886181299797, 81.75501292736983316 ) ) ;
#15381 = CARTESIAN_POINT ( 'NONE',  ( 39.12911128074872380, -29.50384086642191050, 69.06206559358663810 ) ) ;
#15382 = DIRECTION ( 'NONE',  ( -1.000000000000000000, 5.204170427930413997E-31, 1.734723475976804876E-16 ) ) ;
#15383 = CARTESIAN_POINT ( 'NONE',  ( 31.81606138205700418, 41.44123852234595518, 61.30501292736988006 ) ) ;
#15384 = ORIENTED_EDGE ( 'NONE', *, *, #8307, .F. ) ;
#15385 = EDGE_CURVE ( 'NONE', #18741, #131, #20675, .T. ) ;
#15386 = ORIENTED_EDGE ( 'NONE', *, *, #24962, .F. ) ;
#15387 = APPLICATION_CONTEXT ( 'automotive_design' ) ;
#15388 = LINE ( 'NONE', #5354, #22357 ) ;
#15389 = EDGE_CURVE ( 'NONE', #8119, #24709, #13293, .T. ) ;
#15390 = PLANE ( 'NONE',  #16313 ) ;
#15391 = CARTESIAN_POINT ( 'NONE',  ( 39.98359781491296161, -25.20384086642191335, 70.89533451361944572 ) ) ;
#15392 = ADVANCED_FACE ( 'NONE', ( #18743 ), #3530, .T. ) ;
#15393 = CIRCLE ( 'NONE', #4297, 1.749999999999999778 ) ;
#15394 = VECTOR ( 'NONE', #12676, 1000.000000000000000 ) ;
#15395 = FILL_AREA_STYLE_COLOUR ( '', #11293 ) ;
#15396 = DIRECTION ( 'NONE',  ( -0.000000000000000000, -3.469446951953613400E-15, -1.000000000000000000 ) ) ;
#15397 = EDGE_CURVE ( 'NONE', #30, #1030, #9975, .T. ) ;
#15398 = EDGE_CURVE ( 'NONE', #2345, #13616, #25195, .T. ) ;
#15399 = ORIENTED_EDGE ( 'NONE', *, *, #3981, .T. ) ;
#15400 = CARTESIAN_POINT ( 'NONE',  ( 28.81606138205695444, -23.19619402982950263, 47.16846523730000484 ) ) ;
#15401 = VECTOR ( 'NONE', #8045, 1000.000000000000227 ) ;
#15402 = CARTESIAN_POINT ( 'NONE',  ( 36.31606138205700063, 39.69123852234597649, 69.30501292736988717 ) ) ;
#15403 = CARTESIAN_POINT ( 'NONE',  ( 39.81606138205700063, -0.7263636227174442572, 61.39059882987834982 ) ) ;
#15404 = CARTESIAN_POINT ( 'NONE',  ( 37.21915885897815457, -6.203840866421912459, 71.67976084211552745 ) ) ;
#15405 = ORIENTED_EDGE ( 'NONE', *, *, #2468, .F. ) ;
#15406 = ADVANCED_FACE ( 'NONE', ( #15253 ), #11531, .T. ) ;
#15407 = DIRECTION ( 'NONE',  ( 0.000000000000000000, 0.000000000000000000, 1.000000000000000000 ) ) ;
#15408 = ORIENTED_EDGE ( 'NONE', *, *, #5101, .F. ) ;
#15409 = VERTEX_POINT ( 'NONE', #11659 ) ;
#15410 = ADVANCED_FACE ( 'NONE', ( #19618 ), #7786, .T. ) ;
#15411 = DIRECTION ( 'NONE',  ( -0.000000000000000000, 0.7516416929448760387, 0.6595716529892418079 ) ) ;
#15412 = CARTESIAN_POINT ( 'NONE',  ( 39.24876120206128860, -10.71368208888610063, 70.63227792289247020 ) ) ;
#15413 = EDGE_CURVE ( 'NONE', #12829, #22022, #628, .T. ) ;
#15414 = CARTESIAN_POINT ( 'NONE',  ( 39.51027997493896748, -8.513682088886101340, 71.32335560751961623 ) ) ;
#15415 = ORIENTED_EDGE ( 'NONE', *, *, #4067, .F. ) ;
#15416 = ORIENTED_EDGE ( 'NONE', *, *, #11568, .T. ) ;
#15417 = DIRECTION ( 'NONE',  ( -1.000000000000000000, -1.956963323498894821E-16, 5.870889970496684443E-31 ) ) ;
#15418 = CARTESIAN_POINT ( 'NONE',  ( 41.32070064951228971, -37.35828293338759920, 84.30501292737011454 ) ) ;
#15419 = DIRECTION ( 'NONE',  ( 0.000000000000000000, 1.000000000000000000, -3.469446951953614189E-15 ) ) ;
#15420 = CARTESIAN_POINT ( 'NONE',  ( 36.80608444377001831, -16.30384086642191477, 72.40698646996135324 ) ) ;
#15421 = CARTESIAN_POINT ( 'NONE',  ( 41.31606138205700063, 7.864187680719676443, 65.89022736311019912 ) ) ;
#15422 = CARTESIAN_POINT ( 'NONE',  ( 38.00113996487114321, -19.91368208888610170, 72.53360434286904024 ) ) ;
#15423 = AXIS2_PLACEMENT_3D ( 'NONE', #4996, #12861, #20716 ) ;
#15424 = CARTESIAN_POINT ( 'NONE',  ( 43.31606138205700063, -13.58280000135112964, 20.54174511886706256 ) ) ;
#15425 = LINE ( 'NONE', #23274, #7303 ) ;
#15426 = CYLINDRICAL_SURFACE ( 'NONE', #22730, 0.7500000000000031086 ) ;
#15427 = CARTESIAN_POINT ( 'NONE',  ( 39.82611197195675601, -5.853806544725726368, 82.78428315609090760 ) ) ;
#15428 = DIRECTION ( 'NONE',  ( -1.000000000000000000, -2.999999999999999839E-15, 5.603103565922875308E-33 ) ) ;
#15429 = AXIS2_PLACEMENT_3D ( 'NONE', #20862, #24706, #6824 ) ;
#15430 = VECTOR ( 'NONE', #511, 1000.000000000000000 ) ;
#15431 = DIRECTION ( 'NONE',  ( 5.642372883946980038E-32, 1.000000000000000000, -2.848211695852029218E-15 ) ) ;
#15432 = VERTEX_POINT ( 'NONE', #23481 ) ;
#15433 = FACE_OUTER_BOUND ( 'NONE', #18128, .T. ) ;
#15434 = ORIENTED_EDGE ( 'NONE', *, *, #11819, .T. ) ;
#15435 = ORIENTED_EDGE ( 'NONE', *, *, #17196, .T. ) ;
#15436 = CARTESIAN_POINT ( 'NONE',  ( 37.61123632939164452, -11.70384086642191335, 69.02690120949094421 ) ) ;
#15437 = CARTESIAN_POINT ( 'NONE',  ( 40.31606138205701484, -19.68901644060771616, 25.93955620509757409 ) ) ;
#15438 = CARTESIAN_POINT ( 'NONE',  ( 39.95015449827720744, -16.61368208888610454, 70.79240656858105751 ) ) ;
#15439 = ORIENTED_EDGE ( 'NONE', *, *, #17615, .F. ) ;
#15440 = CARTESIAN_POINT ( 'NONE',  ( 46.91606138205695942, 0.06621141594070373282, 0.03267658921017869283 ) ) ;
#15441 = EDGE_CURVE ( 'NONE', #9125, #9136, #165, .T. ) ;
#15442 = DIRECTION ( 'NONE',  ( -1.000000000000000000, -6.505213034913019208E-17, 1.734723475976809806E-16 ) ) ;
#15443 = CARTESIAN_POINT ( 'NONE',  ( 40.77203464402485622, -22.51368208888610667, 71.32335560751960202 ) ) ;
#15444 = EDGE_CURVE ( 'NONE', #23482, #24470, #19064, .T. ) ;
#15445 = VECTOR ( 'NONE', #17515, 1000.000000000000227 ) ;
#15446 = ORIENTED_EDGE ( 'NONE', *, *, #2322, .F. ) ;
#15447 = PRESENTATION_STYLE_ASSIGNMENT (( #13899 ) ) ;
#15448 = CARTESIAN_POINT ( 'NONE',  ( 33.31606138205700773, -4.962695059250739504, 17.19830099227260689 ) ) ;
#15449 = DIRECTION ( 'NONE',  ( 0.000000000000000000, 1.000000000000000000, 0.000000000000000000 ) ) ;
#15450 = PRESENTATION_STYLE_ASSIGNMENT (( #2170 ) ) ;
#15451 = CARTESIAN_POINT ( 'NONE',  ( 43.31606138205700063, 7.043113989679085307, 66.83274420321491505 ) ) ;
#15452 = CARTESIAN_POINT ( 'NONE',  ( 31.81606138205700418, -38.55876147765401640, 70.30501292737012875 ) ) ;
#15453 = CARTESIAN_POINT ( 'NONE',  ( 39.51027997493896748, -11.10384086642191015, 71.43714994484034264 ) ) ;
#15454 = CARTESIAN_POINT ( 'NONE',  ( 39.24876120206128860, -28.71368208888610241, 70.63227792289242757 ) ) ;
#15455 = VERTEX_POINT ( 'NONE', #21186 ) ;
#15456 = CARTESIAN_POINT ( 'NONE',  ( 35.31606138205700773, 1.207247317117632335, 63.73818242441765847 ) ) ;
#15457 = CARTESIAN_POINT ( 'NONE',  ( 33.31606138205700773, -20.26871824316192061, 44.92082169825412308 ) ) ;
#15458 = ORIENTED_EDGE ( 'NONE', *, *, #20566, .T. ) ;
#15459 = ORIENTED_EDGE ( 'NONE', *, *, #23142, .T. ) ;
#15460 = CARTESIAN_POINT ( 'NONE',  ( 40.33642880535521869, -29.30384086642190766, 69.98269868914864844 ) ) ;
#15461 = CARTESIAN_POINT ( 'NONE',  ( 37.60469502381300089, -27.21368208888609885, 70.49320253461758057 ) ) ;
#15462 = CARTESIAN_POINT ( 'NONE',  ( 37.61123632939165873, -1.913682088886106580, 73.73360434286902887 ) ) ;
#15463 = ORIENTED_EDGE ( 'NONE', *, *, #15480, .F. ) ;
#15464 = DIRECTION ( 'NONE',  ( 0.000000000000000000, -2.999999999999999839E-15, -1.000000000000000000 ) ) ;
#15465 = EDGE_CURVE ( 'NONE', #21490, #22425, #15378, .T. ) ;
#15466 = CARTESIAN_POINT ( 'NONE',  ( 37.31647492878124694, -2.303840866421911215, 72.03616607671141026 ) ) ;
#15467 = EDGE_CURVE ( 'NONE', #4631, #24211, #8772, .T. ) ;
#15468 = PRESENTATION_STYLE_ASSIGNMENT (( #3612 ) ) ;
#15469 = VERTEX_POINT ( 'NONE', #1838 ) ;
#15470 = LINE ( 'NONE', #13546, #11752 ) ;
#15471 = DIRECTION ( 'NONE',  ( -1.000000000000000000, -1.000000000000000078E-15, 0.000000000000000000 ) ) ;
#15472 = CARTESIAN_POINT ( 'NONE',  ( 38.37017380507018771, -9.603840866421911926, 69.04448340153881247 ) ) ;
#15473 = LINE ( 'NONE', #15735, #22227 ) ;
#15474 = LINE ( 'NONE', #7887, #3764 ) ;
#15475 = CARTESIAN_POINT ( 'NONE',  ( 40.14115730948191185, -12.51368208888610489, 71.32335560751960202 ) ) ;
#15476 = CARTESIAN_POINT ( 'NONE',  ( 39.31606138205702194, -20.48251210171515879, 31.50167136002490764 ) ) ;
#15477 = FACE_OUTER_BOUND ( 'NONE', #5222, .T. ) ;
#15478 = ORIENTED_EDGE ( 'NONE', *, *, #21408, .F. ) ;
#15479 = CARTESIAN_POINT ( 'NONE',  ( 30.81606138205700418, -26.74044063519544778, 66.30501292737000085 ) ) ;
#15480 = EDGE_CURVE ( 'NONE', #11231, #6167, #3645, .T. ) ;
#15481 = CARTESIAN_POINT ( 'NONE',  ( 39.29254315202757653, -2.803840866421915212, 72.81632618279323310 ) ) ;
#15482 = APPLICATION_PROTOCOL_DEFINITION ( 'draft international standard', 'automotive_design', 1998, #19335 ) ;
#15483 = CARTESIAN_POINT ( 'NONE',  ( 33.31606138205700773, 4.124002793203064066, 6.312068993173404863 ) ) ;
#15484 = CARTESIAN_POINT ( 'NONE',  ( 36.68196826583682935, -17.61368208888610454, 71.96809898377888715 ) ) ;
#15485 = CARTESIAN_POINT ( 'NONE',  ( 40.06606138205700063, 5.308699250829721272, 2.416607620847027960 ) ) ;
#15486 = CARTESIAN_POINT ( 'NONE',  ( 36.68196826583682935, -20.00384086642191050, 70.79240656858107172 ) ) ;
#15487 = CARTESIAN_POINT ( 'NONE',  ( 37.31005363372398165, -5.470823058559972196, 83.30693154845657489 ) ) ;
#15488 = CARTESIAN_POINT ( 'NONE',  ( 36.49096545463212493, -19.51368208888610312, 71.43714994484034264 ) ) ;
#15489 = ORIENTED_EDGE ( 'NONE', *, *, #15075, .F. ) ;
#15490 = CARTESIAN_POINT ( 'NONE',  ( 40.55423172469004811, -20.41368208888610880, 72.05058123536544201 ) ) ;
#15491 = EDGE_LOOP ( 'NONE', ( #2679, #13794, #7839, #17618 ) ) ;
#15492 = LINE ( 'NONE', #21558, #2847 ) ;
#15493 = CARTESIAN_POINT ( 'NONE',  ( 33.31606138205700773, 6.366250835946940967, 6.636353555660927661 ) ) ;
#15494 = CARTESIAN_POINT ( 'NONE',  ( 38.00113996487112189, -21.70384086642190979, 70.22690120949090442 ) ) ;
#15495 = ORIENTED_EDGE ( 'NONE', *, *, #12439, .F. ) ;
#15496 = ORIENTED_EDGE ( 'NONE', *, *, #9857, .T. ) ;
#15497 = CARTESIAN_POINT ( 'NONE',  ( 44.71606138205697079, -4.349482454670842380, -5.142398479549302515 ) ) ;
#15498 = PLANE ( 'NONE',  #5901 ) ;
#15499 = CARTESIAN_POINT ( 'NONE',  ( 45.06606138205697221, -4.349482454670840603, -5.142398479549302515 ) ) ;
#15500 = CARTESIAN_POINT ( 'NONE',  ( 40.33642880535521869, -29.30384086642190766, 69.98269868914864844 ) ) ;
#15501 = DIRECTION ( 'NONE',  ( 1.000000000000000000, -6.938893903907219830E-30, -2.312964634635740294E-15 ) ) ;
#15502 = CARTESIAN_POINT ( 'NONE',  ( 38.26194895904383486, -5.013682088886101340, 69.04448340153881247 ) ) ;
#15503 = LINE ( 'NONE', #11289, #22933 ) ;
#15504 = VECTOR ( 'NONE', #5736, 1000.000000000000114 ) ;
#15505 = ORIENTED_EDGE ( 'NONE', *, *, #15444, .T. ) ;
#15506 = ORIENTED_EDGE ( 'NONE', *, *, #20043, .T. ) ;
#15507 = CIRCLE ( 'NONE', #1505, 2.000000000000001776 ) ;
#15508 = VECTOR ( 'NONE', #18820, 1000.000000000000000 ) ;
#15509 = DIRECTION ( 'NONE',  ( -1.000000000000000000, 6.018531076210110289E-31, 1.734723475976804876E-16 ) ) ;
#15510 = FACE_OUTER_BOUND ( 'NONE', #22927, .T. ) ;
#15511 = EDGE_CURVE ( 'NONE', #24865, #17666, #19240, .T. ) ;
#15512 = CARTESIAN_POINT ( 'NONE',  ( 36.68196826583682935, -26.00384086642191406, 70.79240656858105751 ) ) ;
#15513 = LINE ( 'NONE', #13597, #5062 ) ;
#15514 = SHAPE_REPRESENTATION ( 'Staple Pusher', ( #2000 ), #23998 ) ;
#15515 = ORIENTED_EDGE ( 'NONE', *, *, #10395, .F. ) ;
#15516 = LINE ( 'NONE', #1355, #20112 ) ;
#15517 = DIRECTION ( 'NONE',  ( 2.690219486203388234E-15, -0.8967398287344627850, -0.4425581086832399147 ) ) ;
#15518 = CARTESIAN_POINT ( 'NONE',  ( 41.96606138205694947, 5.208890205473748480, 5.429380561359602453 ) ) ;
#15519 = CARTESIAN_POINT ( 'NONE',  ( 37.69225076346193504, -5.803840866421911215, 70.42958956619168021 ) ) ;
#15520 = ORIENTED_EDGE ( 'NONE', *, *, #8684, .F. ) ;
#15521 = DIRECTION ( 'NONE',  ( -0.1733269559585509378, 0.000000000000000000, -0.9848643390529188135 ) ) ;
#15522 = ORIENTED_EDGE ( 'NONE', *, *, #8106, .T. ) ;
#15523 = ORIENTED_EDGE ( 'NONE', *, *, #4153, .F. ) ;
#15524 = AXIS2_PLACEMENT_3D ( 'NONE', #21024, #23065, #9563 ) ;
#15525 = FACE_OUTER_BOUND ( 'NONE', #14119, .T. ) ;
#15526 = CARTESIAN_POINT ( 'NONE',  ( 39.41296390513587511, -12.41368208888609992, 71.67976084211551324 ) ) ;
#15527 = ADVANCED_FACE ( 'NONE', ( #9473 ), #25144, .F. ) ;
#15528 = VECTOR ( 'NONE', #21038, 1000.000000000000000 ) ;
#15529 = VECTOR ( 'NONE', #3548, 1000.000000000000114 ) ;
#15530 = EDGE_CURVE ( 'NONE', #6472, #23154, #19371, .T. ) ;
#15531 = CARTESIAN_POINT ( 'NONE',  ( 37.89291511884476904, -11.11368208888610276, 70.26206559358664094 ) ) ;
#15532 = ORIENTED_EDGE ( 'NONE', *, *, #14624, .F. ) ;
#15533 = ORIENTED_EDGE ( 'NONE', *, *, #7097, .T. ) ;
#15534 = DIRECTION ( 'NONE',  ( -1.000000000000000000, 0.000000000000000000, 0.000000000000000000 ) ) ;
#15535 = DIRECTION ( 'NONE',  ( 0.000000000000000000, -1.000000000000000000, 2.999999999999999839E-15 ) ) ;
#15536 = CARTESIAN_POINT ( 'NONE',  ( 38.26194895904384907, -18.60384086642191548, 73.11602215082116629 ) ) ;
#15537 = ADVANCED_FACE ( 'NONE', ( #13451 ), #5845, .F. ) ;
#15538 = EDGE_CURVE ( 'NONE', #1971, #3634, #9602, .T. ) ;
#15539 = DIRECTION ( 'NONE',  ( -1.000000000000000000, 0.000000000000000000, 0.000000000000000000 ) ) ;
#15540 = CARTESIAN_POINT ( 'NONE',  ( 37.25260217561390874, -21.61368208888610098, 71.78268878715392987 ) ) ;
#15541 = VERTEX_POINT ( 'NONE', #17451 ) ;
#15542 = CARTESIAN_POINT ( 'NONE',  ( 43.39072112804083758, 3.102161780315297435, 6.136388117020254107 ) ) ;
#15543 = CARTESIAN_POINT ( 'NONE',  ( 39.82603832034401847, -16.31368208888610738, 72.40698646996131060 ) ) ;
#15544 = ADVANCED_FACE ( 'NONE', ( #25277 ), #15498, .T. ) ;
#15545 = DIRECTION ( 'NONE',  ( -1.000000000000000000, 4.513898307157560384E-31, 1.734723475976809806E-16 ) ) ;
#15546 = AXIS2_PLACEMENT_3D ( 'NONE', #6324, #19978, #2189 ) ;
#15547 = CARTESIAN_POINT ( 'NONE',  ( 33.66606138205698073, -5.898435835062239008, -2.003809078978638247 ) ) ;
#15548 = VECTOR ( 'NONE', #5388, 1000.000000000000227 ) ;
#15549 = CARTESIAN_POINT ( 'NONE',  ( 39.91050633825327054, -5.990123355027524354, 83.28119501657926094 ) ) ;
#15550 = DIRECTION ( 'NONE',  ( -1.327674326049719602E-15, 0.4425581086832399147, -0.8967398287344627850 ) ) ;
#15551 = FACE_OUTER_BOUND ( 'NONE', #4540, .T. ) ;
#15552 = ORIENTED_EDGE ( 'NONE', *, *, #284, .T. ) ;
#15553 = CARTESIAN_POINT ( 'NONE',  ( 43.06606138205700063, 41.44123852234595518, 61.30501292736988006 ) ) ;
#15554 = VERTEX_POINT ( 'NONE', #3776 ) ;
#15555 = ORIENTED_EDGE ( 'NONE', *, *, #15832, .F. ) ;
#15556 = CARTESIAN_POINT ( 'NONE',  ( 39.64521430340305841, -8.803840866421916544, 73.30173637941818754 ) ) ;
#15557 = EDGE_LOOP ( 'NONE', ( #18990, #4074, #7959, #982 ) ) ;
#15558 = CARTESIAN_POINT ( 'NONE',  ( 44.81606138205700063, 1.441238522345979600, 68.80501292737000085 ) ) ;
#15559 = CARTESIAN_POINT ( 'NONE',  ( 37.33957961208646736, -11.81368208888610916, 72.81632618279321889 ) ) ;
#15560 = EDGE_CURVE ( 'NONE', #22410, #10213, #5718, .T. ) ;
#15561 = EDGE_CURVE ( 'NONE', #4563, #24251, #18634, .T. ) ;
#15562 = AXIS2_PLACEMENT_3D ( 'NONE', #16826, #20562, #8978 ) ;
#15563 = ORIENTED_EDGE ( 'NONE', *, *, #11969, .T. ) ;
#15564 = CARTESIAN_POINT ( 'NONE',  ( 43.06606138205700063, 41.44123852234599781, 75.30501292736987295 ) ) ;
#15565 = DIRECTION ( 'NONE',  ( 7.071067811865460542E-16, -0.4341746501209495790, -0.9008287146801832179 ) ) ;
#15566 = CARTESIAN_POINT ( 'NONE',  ( 39.64521430340304420, -22.81368208888610383, 69.45876917294175712 ) ) ;
#15567 = ORIENTED_EDGE ( 'NONE', *, *, #19038, .F. ) ;
#15568 = CIRCLE ( 'NONE', #25427, 1.500000000000001332 ) ;
#15569 = DIRECTION ( 'NONE',  ( 1.000000000000000000, -0.000000000000000000, 0.000000000000000000 ) ) ;
#15570 = DIRECTION ( 'NONE',  ( -2.727049986597863807E-15, 0.7516416929448760387, 0.6595716529892418079 ) ) ;
#15571 = DIRECTION ( 'NONE',  ( 1.000000000000000000, 0.000000000000000000, 0.000000000000000000 ) ) ;
#15572 = EDGE_CURVE ( 'NONE', #8707, #5857, #20260, .T. ) ;
#15573 = DIRECTION ( 'NONE',  ( 1.000000000000000000, 0.000000000000000000, 0.000000000000000000 ) ) ;
#15574 = DIRECTION ( 'NONE',  ( 3.469446951953570407E-15, -0.8967398287344626739, -0.4425581086832399702 ) ) ;
#15575 = FACE_BOUND ( 'NONE', #404, .T. ) ;
#15576 = CARTESIAN_POINT ( 'NONE',  ( 39.37952058850012804, -13.00384086642191228, 71.78268878715390144 ) ) ;
#15577 = CARTESIAN_POINT ( 'NONE',  ( 39.31564783533280405, -28.31368208888610383, 72.03616607671136762 ) ) ;
#15578 = CIRCLE ( 'NONE', #13937, 1.500000000000001332 ) ;
#15579 = EDGE_LOOP ( 'NONE', ( #14294, #5742, #11595, #16597 ) ) ;
#15580 = CARTESIAN_POINT ( 'NONE',  ( 39.64097644196145609, -21.75034832497118842, 75.82127938882237572 ) ) ;
#15581 = EDGE_CURVE ( 'NONE', #3785, #19999, #10483, .T. ) ;
#15582 = DIRECTION ( 'NONE',  ( -2.122643018205885151E-17, 1.000000000000000000, -3.120611096041553009E-15 ) ) ;
#15583 = ORIENTED_EDGE ( 'NONE', *, *, #17987, .T. ) ;
#15584 = EDGE_LOOP ( 'NONE', ( #8081, #24261 ) ) ;
#15585 = CARTESIAN_POINT ( 'NONE',  ( 40.26954217208372455, -26.90384086642191619, 72.86986841596730358 ) ) ;
#15586 = AXIS2_PLACEMENT_3D ( 'NONE', #11993, #19697, #484 ) ;
#15587 = CARTESIAN_POINT ( 'NONE',  ( 39.02742774030102879, -26.21368208888610241, 72.26730301774232146 ) ) ;
#15588 = CARTESIAN_POINT ( 'NONE',  ( 37.50301148336529167, -5.113682088886100985, 69.06206559358666652 ) ) ;
#15589 = ORIENTED_EDGE ( 'NONE', *, *, #24809, .F. ) ;
#15590 = CARTESIAN_POINT ( 'NONE',  ( 36.31606138205700063, -7.108955154158179468, 82.62193108360246185 ) ) ;
#15591 = CARTESIAN_POINT ( 'NONE',  ( 37.31647492878124694, -8.303840866421912992, 72.03616607671141026 ) ) ;
#15592 = AXIS2_PLACEMENT_3D ( 'NONE', #15172, #11452, #21108 ) ;
#15593 = DIRECTION ( 'NONE',  ( -1.000000000000000000, 1.115179377413661005E-30, 3.717264591378870232E-16 ) ) ;
#15594 = EDGE_LOOP ( 'NONE', ( #8886, #12255, #10509, #6448 ) ) ;
#15595 = DIRECTION ( 'NONE',  ( 1.000000000000000000, -6.718359089036943783E-31, -1.734723475976804876E-16 ) ) ;
#15596 = FACE_OUTER_BOUND ( 'NONE', #1036, .T. ) ;
#15597 = CARTESIAN_POINT ( 'NONE',  ( 36.11133435605973574, -12.00384086642191583, 70.60699637195608602 ) ) ;
#15598 = CARTESIAN_POINT ( 'NONE',  ( 46.81606138205697221, -5.918777154956146980, -5.916875169744970187 ) ) ;
#15599 = VECTOR ( 'NONE', #23599, 1000.000000000000000 ) ;
#15600 = SURFACE_SIDE_STYLE ('',( #1678 ) ) ;
#15601 = CARTESIAN_POINT ( 'NONE',  ( 37.69796330110504101, -15.11368208888609743, 69.66206559358661821 ) ) ;
#15602 = DIRECTION ( 'NONE',  ( 1.000000000000000000, 0.000000000000000000, 0.000000000000000000 ) ) ;
#15603 = FACE_OUTER_BOUND ( 'NONE', #1255, .T. ) ;
#15604 = VECTOR ( 'NONE', #20705, 1000.000000000000000 ) ;
#15605 = EDGE_LOOP ( 'NONE', ( #16495, #9782, #1603, #24137 ) ) ;
#15606 = CARTESIAN_POINT ( 'NONE',  ( 43.81606138205700063, -27.66931681479738003, 59.51410614687260647 ) ) ;
#15607 = CARTESIAN_POINT ( 'NONE',  ( 40.14115730948191185, -5.103840866421911038, 71.43714994484034264 ) ) ;
#15608 = ADVANCED_FACE ( 'NONE', ( #13957 ), #10222, .T. ) ;
#15609 = CARTESIAN_POINT ( 'NONE',  ( 33.34326309846886005, 3.870673299598025086, 6.311734371576938507 ) ) ;
#15610 = AXIS2_PLACEMENT_3D ( 'NONE', #20951, #15271, #24908 ) ;
#15611 = CARTESIAN_POINT ( 'NONE',  ( 36.64852494920107517, -21.41368208888610525, 70.89533451361947414 ) ) ;
#15612 = EDGE_CURVE ( 'NONE', #20448, #10061, #6229, .T. ) ;
#15613 = VECTOR ( 'NONE', #8491, 1000.000000000000000 ) ;
#15614 = DIRECTION ( 'NONE',  ( 1.000000000000000000, 0.000000000000000000, 0.000000000000000000 ) ) ;
#15615 = EDGE_CURVE ( 'NONE', #4487, #22083, #14121, .T. ) ;
#15616 = CARTESIAN_POINT ( 'NONE',  ( 39.95015449827720744, -15.00384086642191228, 71.96809898377887293 ) ) ;
#15617 = CARTESIAN_POINT ( 'NONE',  ( 38.31606138205700063, -6.549308025893449070, 20.35783565644092619 ) ) ;
#15618 = AXIS2_PLACEMENT_3D ( 'NONE', #9277, #16861, #11200 ) ;
#15619 = CARTESIAN_POINT ( 'NONE',  ( 36.64852494920107517, -19.41368208888610525, 70.89533451361947414 ) ) ;
#15620 = EDGE_LOOP ( 'NONE', ( #442, #18018, #13444, #19517 ) ) ;
#15621 = CARTESIAN_POINT ( 'NONE',  ( 36.07789103942398867, -19.41368208888610525, 70.70992431699450265 ) ) ;
#15622 = VERTEX_POINT ( 'NONE', #21940 ) ;
#15623 = DIRECTION ( 'NONE',  ( -1.000000000000000000, 5.630462536178272263E-31, 8.673617379884039170E-17 ) ) ;
#15624 = DIRECTION ( 'NONE',  ( -1.000000000000000000, 1.115179377413661005E-30, 3.717264591378870232E-16 ) ) ;
#15625 = CARTESIAN_POINT ( 'NONE',  ( 37.21915885897815457, -24.20384086642190979, 71.67976084211551324 ) ) ;
#15626 = VECTOR ( 'NONE', #3039, 1000.000000000000000 ) ;
#15627 = ORIENTED_EDGE ( 'NONE', *, *, #5032, .T. ) ;
#15628 = VECTOR ( 'NONE', #6222, 1000.000000000000000 ) ;
#15629 = ORIENTED_EDGE ( 'NONE', *, *, #23724, .T. ) ;
#15630 = CARTESIAN_POINT ( 'NONE',  ( 40.31606138205700773, -18.80550481115971095, 25.27912300651437150 ) ) ;
#15631 = EDGE_CURVE ( 'NONE', #16802, #13184, #16261, .T. ) ;
#15632 = DIRECTION ( 'NONE',  ( 1.000000000000000000, 2.827156040805656045E-15, -8.530177117963464484E-17 ) ) ;
#15633 = VERTEX_POINT ( 'NONE', #22060 ) ;
#15634 = CARTESIAN_POINT ( 'NONE',  ( 43.31606138205700063, -27.52349462642295208, 56.67559192035834315 ) ) ;
#15635 = CARTESIAN_POINT ( 'NONE',  ( 40.77203464402485622, -27.10384086642191903, 71.43714994484031422 ) ) ;
#15636 = CIRCLE ( 'NONE', #4534, 4.000000000000000000 ) ;
#15637 = LINE ( 'NONE', #1708, #18296 ) ;
#15638 = CARTESIAN_POINT ( 'NONE',  ( 40.77203464402485622, -0.5136820888861047818, 71.32335560751961623 ) ) ;
#15639 = VECTOR ( 'NONE', #21787, 1000.000000000000000 ) ;
#15640 = FACE_OUTER_BOUND ( 'NONE', #11794, .T. ) ;
#15641 = ORIENTED_EDGE ( 'NONE', *, *, #17759, .T. ) ;
#15642 = ORIENTED_EDGE ( 'NONE', *, *, #14426, .F. ) ;
#15643 = CARTESIAN_POINT ( 'NONE',  ( 32.81606138205700773, 41.44123852234598360, 71.05501292736988717 ) ) ;
#15644 = CARTESIAN_POINT ( 'NONE',  ( 36.64852494920107517, -18.20384086642191335, 71.86517103874048473 ) ) ;
#15645 = CARTESIAN_POINT ( 'NONE',  ( 30.81606138205700418, 40.39281886181299797, 84.30501292736984453 ) ) ;
#15646 = ORIENTED_EDGE ( 'NONE', *, *, #2009, .T. ) ;
#15647 = AXIS2_PLACEMENT_3D ( 'NONE', #18704, #2839, #20507 ) ;
#15648 = DIRECTION ( 'NONE',  ( -1.000000000000000000, -1.052872940142565459E-15, -1.848188032574765003E-17 ) ) ;
#15649 = VECTOR ( 'NONE', #19173, 1000.000000000000000 ) ;
#15650 = LINE ( 'NONE', #3541, #16433 ) ;
#15651 = DIRECTION ( 'NONE',  ( 1.000000000000000000, 1.000000000000000078E-15, 0.000000000000000000 ) ) ;
#15652 = CARTESIAN_POINT ( 'NONE',  ( 39.02742774030101458, -7.403840866421910860, 70.49320253461759478 ) ) ;
#15653 = VERTEX_POINT ( 'NONE', #23737 ) ;
#15654 = DIRECTION ( 'NONE',  ( 1.327674326049719602E-15, -0.4425581086832399147, 0.8967398287344627850 ) ) ;
#15655 = VERTEX_POINT ( 'NONE', #4424 ) ;
#15656 = ORIENTED_EDGE ( 'NONE', *, *, #2457, .T. ) ;
#15657 = DIRECTION ( 'NONE',  ( 1.734723475976804876E-16, 3.269436733918100469E-15, 1.000000000000000000 ) ) ;
#15658 = CARTESIAN_POINT ( 'NONE',  ( 37.31647492878122563, -15.31368208888610205, 70.72433947564853440 ) ) ;
#15659 = CARTESIAN_POINT ( 'NONE',  ( 38.37017380507020192, -14.01368208888610312, 72.51602215082118619 ) ) ;
#15660 = ORIENTED_EDGE ( 'NONE', *, *, #3487, .F. ) ;
#15661 = VERTEX_POINT ( 'NONE', #6479 ) ;
#15662 = FACE_OUTER_BOUND ( 'NONE', #6250, .T. ) ;
#15663 = EDGE_CURVE ( 'NONE', #22, #12724, #20135, .T. ) ;
#15664 = DIRECTION ( 'NONE',  ( 1.000000000000000000, 1.159780179694326360E-16, 8.617271610285116919E-17 ) ) ;
#15665 = ORIENTED_EDGE ( 'NONE', *, *, #19863, .T. ) ;
#15666 = CARTESIAN_POINT ( 'NONE',  ( 38.93415946300897446, 1.886317911113891244, 73.09843995877332645 ) ) ;
#15667 = CARTESIAN_POINT ( 'NONE',  ( 40.14115730948191185, -15.10384086642190837, 71.43714994484030001 ) ) ;
#15668 = AXIS2_PLACEMENT_3D ( 'NONE', #22408, #14549, #7074 ) ;
#15669 = CARTESIAN_POINT ( 'NONE',  ( 42.82259739205072435, 3.224889171211050343, 6.370942055173422602 ) ) ;
#15670 = PLANE ( 'NONE',  #7534 ) ;
#15671 = CARTESIAN_POINT ( 'NONE',  ( 37.21915885897815457, -19.41368208888609814, 71.08074471024443142 ) ) ;
#15672 = ORIENTED_EDGE ( 'NONE', *, *, #15707, .T. ) ;
#15673 = AXIS2_PLACEMENT_3D ( 'NONE', #6500, #19776, #4064 ) ;
#15674 = VERTEX_POINT ( 'NONE', #4675 ) ;
#15675 =( BOUNDED_CURVE ( )  B_SPLINE_CURVE ( 2, ( #13464, #9240, #25290, #17086, #22991, #21316, #22868, #3658, #9110, #1717, #11543, #9360, #25030, #25156, #5227, #7546, #1476, #7669, #5480, #5729, #23241, #5604, #13224, #19255, #13090, #23114, #7288, #11025, #15136, #7418, #20819, #1593, #15512, #5357, #21073, #9483, #23364, #21197, #17331, #3153, #15391, #18883, #11412, #16950, #3417, #11296, #3536, #19139, #21698, #45, #15893, #19764, #174, #10113, #11798, #1974, #21952, #418, #13596, #5990, #2237, #16142, #12181, #21445, #6239, #3789, #7928, #14097, #15774, #11673, #9858, #19898, #5862, #9985, #12052, #16017, #17971, #21823, #19633, #8302, #17716, #23632, #8175, #17587, #296, #4315, #19513, #23996, #21577, #13843, #11923, #23867, #1851, #2104, #4049, #23493, #17848, #8052, #23750, #6111, #13970, #4183, #9733, #20019, #25414, #2357, #10234, #18100, #7797, #13721, #15644, #3927, #8935, #6863, #18467, #22201, #16521, #4802, #24370, #12565, #12684, #4437, #4687, #2610, #16271, #24241, #8558, #20397, #671, #6746, #8689, #20524, #10493, #18724, #10748, #6613, #20654, #2728, #16659, #4938, #22331, #1058, #10619, #16784, #14229, #929, #803, #6373, #18347, #12303, #16393, #14596, #22072, #20149, #24488, #20273, #10873, #14348, #14474, #14720, #8433, #8821, #24114, #22454, #2990, #12806, #6492, #18591, #2484, #2857, #10356, #18221, #22581, #550, #4567, #12434, #17050, #23079, #16920, #19109, #10992, #22837, #24876, #7128, #11510, #1561, #19351, #13433, #14983, #3123, #5070, #15356, #7255, #1446, #5198, #24615, #15229, #9577, #24750, #9076, #17173, #3381, #5444, #18978, #15102, #3246, #12935, #13057, #9329, #3626, #22962, #20912, #21282, #11127, #1318, #1684, #23206, #6998, #17301, #14847, #9205, #20788, #22706, #13314, #24998, #1186, #21166, #18846, #5324, #13187, #21039, #11260, #7385, #19221, #3506, #11379, #9452, #25122, #5574, #7503, #2324, #15607, #2205, #9827, #15863, #9704, #11891, #3756, #7638, #11636, #4017, #17426, #23714, #23837, #1817, #3892, #6080, #6209, #9953, #13939, #259, #25380, #25256, #8025, #15481, #17554, #7763, #17814, #19732, #12, #11766, #2074, #23595, #146, #21795, #23463, #5827, #8137, #4281, #23328, #17681, #19600, #19989, #15981, #5694, #10084, #13558, #1941, #17943, #7894, #21413, #13687, #4154, #21546, #13809, #12021, #19861, #14065, #21919, #15741, #12152, #19474, #5959, #21663, #14198, #24690, #3188 ),
 .UNSPECIFIED., .F., .T. ) 
 B_SPLINE_CURVE_WITH_KNOTS ( ( 3, 2, 2, 2, 2, 2, 2, 2, 2, 2, 2, 2, 2, 2, 2, 2, 2, 2, 2, 2, 2, 2, 2, 2, 2, 2, 2, 2, 2, 2, 2, 2, 2, 2, 2, 2, 2, 2, 2, 2, 2, 2, 2, 2, 2, 2, 2, 2, 2, 2, 2, 2, 2, 2, 2, 2, 2, 2, 2, 2, 2, 2, 2, 2, 2, 2, 2, 2, 2, 2, 2, 2, 2, 2, 2, 2, 2, 2, 2, 2, 2, 2, 2, 2, 2, 2, 2, 2, 2, 2, 2, 2, 2, 2, 2, 2, 2, 2, 2, 2, 2, 2, 2, 2, 2, 2, 2, 2, 2, 2, 2, 2, 2, 2, 2, 2, 2, 2, 2, 2, 2, 2, 2, 2, 2, 2, 2, 2, 2, 2, 2, 2, 2, 2, 2, 2, 2, 2, 2, 2, 2, 2, 2, 2, 2, 2, 2, 2, 2, 2, 2, 2, 2, 3 ),
 ( 0.01547498522512168184, 0.01874999999999999931, 0.02500000000000000139, 0.03125000000000000000, 0.03749999999999999861, 0.04374999999999999722, 0.05000000000000000278, 0.05625000000000000139, 0.06250000000000000000, 0.06875000000000000555, 0.07499999999999999722, 0.08125000000000000278, 0.08749999999999999445, 0.09375000000000000000, 0.1000000000000000056, 0.1062499999999999972, 0.1125000000000000028, 0.1187499999999999944, 0.1250000000000000000, 0.1312500000000000056, 0.1375000000000000111, 0.1437499999999999889, 0.1500000000000000222, 0.1562500000000000000, 0.1625000000000000333, 0.1687500000000000111, 0.1749999999999999889, 0.1812500000000000222, 0.1875000000000000000, 0.1937500000000000333, 0.2000000000000000111, 0.2062499999999999889, 0.2125000000000000222, 0.2187500000000000000, 0.2250000000000000333, 0.2312500000000000111, 0.2374999999999999889, 0.2437500000000000222, 0.2500000000000000000, 0.2562499999999999778, 0.2625000000000000111, 0.2687499999999999889, 0.2750000000000000222, 0.2812500000000000000, 0.2874999999999999778, 0.2937500000000000111, 0.2999999999999999889, 0.3062500000000000222, 0.3125000000000000000, 0.3187499999999999778, 0.3250000000000000111, 0.3312499999999999889, 0.3375000000000000222, 0.3437500000000000000, 0.3499999999999999778, 0.3562500000000000111, 0.3624999999999999889, 0.3687500000000000222, 0.3750000000000000000, 0.3812499999999999778, 0.3875000000000000111, 0.3937499999999999889, 0.4000000000000000222, 0.4062500000000000000, 0.4124999999999999778, 0.4187500000000000111, 0.4249999999999999889, 0.4312500000000000222, 0.4375000000000000000, 0.4437499999999999778, 0.4500000000000000111, 0.4562499999999999889, 0.4625000000000000222, 0.4687500000000000000, 0.4749999999999999778, 0.4812500000000000111, 0.4874999999999999889, 0.4937500000000000222, 0.5000000000000000000, 0.5062499999999999778, 0.5124999999999999556, 0.5187500000000000444, 0.5250000000000000222, 0.5312500000000000000, 0.5374999999999999778, 0.5437499999999999556, 0.5500000000000000444, 0.5562500000000000222, 0.5625000000000000000, 0.5687499999999999778, 0.5749999999999999556, 0.5812500000000000444, 0.5875000000000000222, 0.5937500000000000000, 0.5999999999999999778, 0.6062499999999999556, 0.6125000000000000444, 0.6187500000000000222, 0.6250000000000000000, 0.6312499999999999778, 0.6374999999999999556, 0.6437500000000000444, 0.6500000000000000222, 0.6562500000000000000, 0.6624999999999999778, 0.6687499999999999556, 0.6750000000000001554, 0.6812500000000000222, 0.6875000000000000000, 0.6937499999999999778, 0.6999999999999999556, 0.7062500000000000444, 0.7125000000000000222, 0.7187500000000000000, 0.7249999999999999778, 0.7312499999999999556, 0.7375000000000000444, 0.7437500000000000222, 0.7500000000000000000, 0.7562499999999999778, 0.7624999999999999556, 0.7687500000000000444, 0.7750000000000001332, 0.7812500000000000000, 0.7874999999999999778, 0.7937499999999999556, 0.8000000000000000444, 0.8062500000000000222, 0.8125000000000000000, 0.8187499999999999778, 0.8249999999999999556, 0.8312500000000000444, 0.8375000000000000222, 0.8437500000000000000, 0.8499999999999999778, 0.8562499999999999556, 0.8625000000000000444, 0.8687500000000000222, 0.8750000000000000000, 0.8812499999999999778, 0.8874999999999999556, 0.8937500000000000444, 0.9000000000000000222, 0.9062500000000000000, 0.9124999999999999778, 0.9187499999999999556, 0.9250000000000001554, 0.9312500000000000222, 0.9375000000000000000, 0.9437499999999999778, 0.9499999999999999556, 0.9562500000000000444, 0.9625000000000000222, 0.9687500000000000000 ),
 .UNSPECIFIED. ) 
 CURVE ( )  GEOMETRIC_REPRESENTATION_ITEM ( )  RATIONAL_B_SPLINE_CURVE ( ( 0.9755846521486901679, 0.9743534988372177796, 1.000000000000000000, 0.9510565162951535312, 1.000000000000000000, 0.9510565162951535312, 1.000000000000000000, 0.9510565162951535312, 1.000000000000000000, 0.9510565162951535312, 1.000000000000000000, 0.9510565162951535312, 1.000000000000000000, 0.9510565162951535312, 1.000000000000000000, 0.9510565162951535312, 1.000000000000000000, 0.9510565162951535312, 1.000000000000000000, 0.9510565162951535312, 1.000000000000000000, 0.9510565162951535312, 1.000000000000000000, 0.9510565162951535312, 1.000000000000000000, 0.9510565162951535312, 1.000000000000000000, 0.9510565162951535312, 1.000000000000000000, 0.9510565162951535312, 1.000000000000000000, 0.9510565162951535312, 1.000000000000000000, 0.9510565162951535312, 1.000000000000000000, 0.9510565162951535312, 1.000000000000000000, 0.9510565162951535312, 1.000000000000000000, 0.9510565162951535312, 1.000000000000000000, 0.9510565162951535312, 1.000000000000000000, 0.9510565162951535312, 1.000000000000000000, 0.9510565162951535312, 1.000000000000000000, 0.9510565162951535312, 1.000000000000000000, 0.9510565162951535312, 1.000000000000000000, 0.9510565162951535312, 1.000000000000000000, 0.9510565162951535312, 1.000000000000000000, 0.9510565162951535312, 1.000000000000000000, 0.9510565162951535312, 1.000000000000000000, 0.9510565162951535312, 1.000000000000000000, 0.9510565162951535312, 1.000000000000000000, 0.9510565162951535312, 1.000000000000000000, 0.9510565162951535312, 1.000000000000000000, 0.9510565162951535312, 1.000000000000000000, 0.9510565162951535312, 1.000000000000000000, 0.9510565162951535312, 1.000000000000000000, 0.9510565162951535312, 1.000000000000000000, 0.9510565162951535312, 1.000000000000000000, 0.9510565162951535312, 1.000000000000000000, 0.9510565162951535312, 1.000000000000000000, 0.9510565162951535312, 1.000000000000000000, 0.9510565162951535312, 1.000000000000000000, 0.9510565162951535312, 1.000000000000000000, 0.9510565162951535312, 1.000000000000000000, 0.9510565162951535312, 1.000000000000000000, 0.9510565162951535312, 1.000000000000000000, 0.9510565162951535312, 1.000000000000000000, 0.9510565162951535312, 1.000000000000000000, 0.9510565162951535312, 1.000000000000000000, 0.9510565162951535312, 1.000000000000000000, 0.9510565162951535312, 1.000000000000000000, 0.9510565162951535312, 1.000000000000000000, 0.9510565162951535312, 1.000000000000000000, 0.9510565162951535312, 1.000000000000000000, 0.9510565162951535312, 1.000000000000000000, 0.9510565162951535312, 1.000000000000000000, 0.9510565162951535312, 1.000000000000000000, 0.9510565162951535312, 1.000000000000000000, 0.9510565162951535312, 1.000000000000000000, 0.9510565162951535312, 1.000000000000000000, 0.9510565162951535312, 1.000000000000000000, 0.9510565162951535312, 1.000000000000000000, 0.9510565162951535312, 1.000000000000000000, 0.9510565162951535312, 1.000000000000000000, 0.9510565162951535312, 1.000000000000000000, 0.9510565162951535312, 1.000000000000000000, 0.9510565162951535312, 1.000000000000000000, 0.9510565162951535312, 1.000000000000000000, 0.9510565162951535312, 1.000000000000000000, 0.9510565162951535312, 1.000000000000000000, 0.9510565162951535312, 1.000000000000000000, 0.9510565162951535312, 1.000000000000000000, 0.9510565162951535312, 1.000000000000000000, 0.9510565162951535312, 1.000000000000000000, 0.9510565162951535312, 1.000000000000000000, 0.9510565162951535312, 1.000000000000000000, 0.9510565162951535312, 1.000000000000000000, 0.9510565162951535312, 1.000000000000000000, 0.9510565162951535312, 1.000000000000000000, 0.9510565162951535312, 1.000000000000000000, 0.9510565162951535312, 1.000000000000000000, 0.9510565162951535312, 1.000000000000000000, 0.9510565162951535312, 1.000000000000000000, 0.9510565162951535312, 1.000000000000000000, 0.9510565162951535312, 1.000000000000000000, 0.9510565162951535312, 1.000000000000000000, 0.9510565162951535312, 1.000000000000000000, 0.9510565162951535312, 1.000000000000000000, 0.9510565162951535312, 1.000000000000000000, 0.9510565162951535312, 1.000000000000000000, 0.9510565162951535312, 1.000000000000000000, 0.9510565162951535312, 1.000000000000000000, 0.9510565162951535312, 1.000000000000000000, 0.9510565162951535312, 1.000000000000000000, 0.9510565162951535312, 1.000000000000000000, 0.9510565162951535312, 1.000000000000000000, 0.9510565162951535312, 1.000000000000000000, 0.9510565162951535312, 1.000000000000000000, 0.9510565162951535312, 1.000000000000000000, 0.9510565162951535312, 1.000000000000000000, 0.9510565162951535312, 1.000000000000000000, 0.9510565162951535312, 1.000000000000000000, 0.9510565162951535312, 1.000000000000000000, 0.9510565162951535312, 1.000000000000000000, 0.9510565162951535312, 1.000000000000000000, 0.9510565162951535312, 1.000000000000000000, 0.9510565162951535312, 1.000000000000000000, 0.9510565162951535312, 1.000000000000000000, 0.9510565162951535312, 1.000000000000000000, 0.9510565162951535312, 1.000000000000000000, 0.9510565162951535312, 1.000000000000000000, 0.9510565162951535312, 1.000000000000000000, 0.9510565162951535312, 1.000000000000000000, 0.9510565162951535312, 1.000000000000000000, 0.9510565162951535312, 1.000000000000000000, 0.9510565162951535312, 1.000000000000000000, 0.9510565162951535312, 1.000000000000000000, 0.9510565162951535312, 1.000000000000000000, 0.9510565162951535312, 1.000000000000000000, 0.9510565162951535312, 1.000000000000000000, 0.9510565162951535312, 1.000000000000000000, 0.9510565162951535312, 1.000000000000000000, 0.9510565162951535312, 1.000000000000000000, 0.9510565162951535312, 1.000000000000000000, 0.9510565162951535312, 1.000000000000000000, 0.9510565162951535312, 1.000000000000000000, 0.9510565162951535312, 1.000000000000000000, 0.9510565162951535312, 1.000000000000000000, 0.9510565162951535312, 1.000000000000000000, 0.9510565162951535312, 1.000000000000000000, 0.9510565162951535312, 1.000000000000000000, 0.9510565162951535312, 1.000000000000000000, 0.9510565162951535312, 1.000000000000000000, 0.9510565162951535312, 1.000000000000000000, 0.9510565162951535312, 1.000000000000000000, 0.9510565162951535312, 1.000000000000000000, 0.9510565162951535312, 1.000000000000000000, 0.9510565162951535312, 1.000000000000000000, 0.9510565162951535312, 1.000000000000000000, 0.9510565162951535312, 1.000000000000000000, 0.9510565162951535312, 1.000000000000000000, 0.9510565162951535312, 1.000000000000000000, 0.9510565162951535312, 1.000000000000000000, 0.9510565162951535312, 1.000000000000000000, 0.9510565162951535312, 1.000000000000000000, 0.9510565162951535312, 1.000000000000000000, 0.9510565162951535312, 1.000000000000000000, 0.9510565162951535312, 1.000000000000000000, 0.9510565162951535312, 1.000000000000000000, 0.9510565162951535312, 1.000000000000000000, 0.9510565162951535312, 1.000000000000000000, 0.9510565162951535312, 1.000000000000000000, 0.9510565162951535312, 1.000000000000000000 ) ) 
 REPRESENTATION_ITEM ( '' )  );
#15676 = CARTESIAN_POINT ( 'NONE',  ( 30.81606138205696155, -0.2703287878658127696, 1.505452687840413972 ) ) ;
#15677 = CARTESIAN_POINT ( 'NONE',  ( 36.80608444377001121, -13.31368208888609850, 70.35351908239860563 ) ) ;
#15678 = LINE ( 'NONE', #2267, #16758 ) ;
#15679 = CARTESIAN_POINT ( 'NONE',  ( 43.31606138205700063, -20.88462213363798270, 44.49284693533410717 ) ) ;
#15680 = CARTESIAN_POINT ( 'NONE',  ( 38.26194895904383486, -29.01368208888610312, 69.64448340153876416 ) ) ;
#15681 = LINE ( 'NONE', #23528, #21750 ) ;
#15682 = B_SPLINE_SURFACE_WITH_KNOTS ( 'NONE', 1, 3, ( 
 ( #18286, #12229, #23802, #4366 ),
 ( #2166, #19953, #14277, #8615 ),
 ( #21885, #18402, #350, #14163 ) ),
 .UNSPECIFIED., .F., .F., .F.,
 ( 2, 1, 2 ),
 ( 4, 4 ),
 ( -0.01000000000000000021, 0.000000000000000000, 1.000000000000000000 ),
 ( 0.000000000000000000, 1.000000000000000000 ),
 .UNSPECIFIED. ) ;
#15683 = DIRECTION ( 'NONE',  ( 0.000000000000000000, 2.999999999999999839E-15, 1.000000000000000000 ) ) ;
#15684 = ORIENTED_EDGE ( 'NONE', *, *, #3412, .T. ) ;
#15685 = DIRECTION ( 'NONE',  ( 1.734723475976804876E-16, 3.491481338843135327E-15, 1.000000000000000000 ) ) ;
#15686 = ORIENTED_EDGE ( 'NONE', *, *, #7660, .F. ) ;
#15687 = EDGE_LOOP ( 'NONE', ( #20543, #23299 ) ) ;
#15688 = CIRCLE ( 'NONE', #4594, 0.7500000000000021094 ) ;
#15689 = CARTESIAN_POINT ( 'NONE',  ( 38.37017380507018771, -1.603840866421912148, 69.04448340153881247 ) ) ;
#15690 = ORIENTED_EDGE ( 'NONE', *, *, #20148, .T. ) ;
#15691 = EDGE_CURVE ( 'NONE', #6977, #11231, #4306, .T. ) ;
#15692 = CARTESIAN_POINT ( 'NONE',  ( 40.81606138205700773, 37.44123852234599781, 75.30501292736990138 ) ) ;
#15693 = CARTESIAN_POINT ( 'NONE',  ( 40.14115730948191185, -14.51368208888610667, 71.32335560751960202 ) ) ;
#15694 = FILL_AREA_STYLE_COLOUR ( '', #10433 ) ;
#15695 = ORIENTED_EDGE ( 'NONE', *, *, #11804, .F. ) ;
#15696 = CARTESIAN_POINT ( 'NONE',  ( 43.81606138205700063, 2.191238522347000117, 69.30501292737000085 ) ) ;
#15697 = PLANE ( 'NONE',  #21161 ) ;
#15698 = CARTESIAN_POINT ( 'NONE',  ( 40.26954217208371034, -12.71368208888610241, 69.89063713639258424 ) ) ;
#15699 = ORIENTED_EDGE ( 'NONE', *, *, #13511, .F. ) ;
#15700 = CARTESIAN_POINT ( 'NONE',  ( 44.06606138205700063, -26.74044063519535186, 82.55501292737007191 ) ) ;
#15701 = CIRCLE ( 'NONE', #6263, 0.9023161253044892360 ) ;
#15702 = CARTESIAN_POINT ( 'NONE',  ( 31.81606138205700418, -34.55876147765410167, 70.30501292737000085 ) ) ;
#15703 = EDGE_CURVE ( 'NONE', #3936, #10892, #18089, .T. ) ;
#15704 = ADVANCED_FACE ( 'NONE', ( #23984 ), #538, .F. ) ;
#15705 = DIRECTION ( 'NONE',  ( 1.000000000000000000, 2.973811673103095397E-15, 0.000000000000000000 ) ) ;
#15706 = AXIS2_PLACEMENT_3D ( 'NONE', #24608, #16912, #24741 ) ;
#15707 = EDGE_CURVE ( 'NONE', #19809, #3263, #11666, .T. ) ;
#15708 = CYLINDRICAL_SURFACE ( 'NONE', #24407, 0.5000000000000011102 ) ;
#15709 = EDGE_CURVE ( 'NONE', #13733, #8317, #23856, .T. ) ;
#15710 = CARTESIAN_POINT ( 'NONE',  ( 38.73920764526923932, -15.50384086642191228, 70.26206559358661252 ) ) ;
#15711 = CARTESIAN_POINT ( 'NONE',  ( 36.68196826583682935, -1.613682088886104982, 71.96809898377890136 ) ) ;
#15712 = EDGE_CURVE ( 'NONE', #6422, #18550, #8291, .T. ) ;
#15713 = ORIENTED_EDGE ( 'NONE', *, *, #15560, .T. ) ;
#15714 = CARTESIAN_POINT ( 'NONE',  ( 38.31606138205700063, -22.22127907754186893, 75.81001292736998209 ) ) ;
#15715 = FACE_OUTER_BOUND ( 'NONE', #18324, .T. ) ;
#15716 = ORIENTED_EDGE ( 'NONE', *, *, #4379, .F. ) ;
#15717 = ORIENTED_EDGE ( 'NONE', *, *, #5792, .T. ) ;
#15718 = CARTESIAN_POINT ( 'NONE',  ( 39.75915168707251723, -0.9038408664219161892, 72.49904802271740323 ) ) ;
#15719 = ADVANCED_FACE ( 'NONE', ( #8546 ), #20388, .T. ) ;
#15720 = CARTESIAN_POINT ( 'NONE',  ( 38.93987200065208754, -22.81368208888610383, 70.42958956619168021 ) ) ;
#15721 = CARTESIAN_POINT ( 'NONE',  ( 36.89935272106204422, -1.213682088886100630, 69.52238214136768590 ) ) ;
#15722 = AXIS2_PLACEMENT_3D ( 'NONE', #23658, #15801, #8332 ) ;
#15723 = ORIENTED_EDGE ( 'NONE', *, *, #3442, .F. ) ;
#15724 = DIRECTION ( 'NONE',  ( 0.000000000000000000, -2.999999999999999839E-15, -1.000000000000000000 ) ) ;
#15725 = EDGE_CURVE ( 'NONE', #14027, #6661, #16379, .T. ) ;
#15726 = VECTOR ( 'NONE', #15809, 1000.000000000000000 ) ;
#15727 = CARTESIAN_POINT ( 'NONE',  ( 40.14115730948191185, -27.10384086642190482, 71.43714994484028580 ) ) ;
#15728 = APPLICATION_CONTEXT ( 'automotive_design' ) ;
#15729 = DIRECTION ( 'NONE',  ( 0.000000000000000000, 0.000000000000000000, 1.000000000000000000 ) ) ;
#15730 = ORIENTED_EDGE ( 'NONE', *, *, #15930, .T. ) ;
#15731 = LINE ( 'NONE', #7491, #17080 ) ;
#15732 = DIRECTION ( 'NONE',  ( -1.000000000000000000, 0.000000000000000000, 0.000000000000000000 ) ) ;
#15733 = CIRCLE ( 'NONE', #15303, 0.2000000000000057288 ) ;
#15734 = CARTESIAN_POINT ( 'NONE',  ( 38.26194895904384197, -12.60384086642191903, 73.71602215082113219 ) ) ;
#15735 = CARTESIAN_POINT ( 'NONE',  ( 30.81606138205700418, 36.92314894770294131, 80.37823623207323465 ) ) ;
#15736 = CARTESIAN_POINT ( 'NONE',  ( 39.82603832034400426, -14.31368208888610916, 72.40698646996133903 ) ) ;
#15737 = FACE_OUTER_BOUND ( 'NONE', #14040, .T. ) ;
#15738 = AXIS2_PLACEMENT_3D ( 'NONE', #1647, #9793, #19433 ) ;
#15739 = CARTESIAN_POINT ( 'NONE',  ( 38.26194895904383486, -25.01368208888610312, 69.64448340153876416 ) ) ;
#15740 = FACE_OUTER_BOUND ( 'NONE', #17226, .T. ) ;
#15741 = CARTESIAN_POINT ( 'NONE',  ( 39.82603832034401137, 0.6961591335780912271, 70.35351908239861984 ) ) ;
#15742 = CONTEXT_DEPENDENT_SHAPE_REPRESENTATION ( #24095, #20012 ) ;
#15743 = AXIS2_PLACEMENT_3D ( 'NONE', #11799, #15396, #19636 ) ;
#15744 = DIRECTION ( 'NONE',  ( -1.000000000000000000, -1.000000000000000078E-15, 0.000000000000000000 ) ) ;
#15745 = CARTESIAN_POINT ( 'NONE',  ( 37.25202387243752611, -19.21368208888610241, 70.00779233799262613 ) ) ;
#15746 = CARTESIAN_POINT ( 'NONE',  ( 43.31606138205700773, -19.13113579875041381, 24.60350147050422720 ) ) ;
#15747 = CARTESIAN_POINT ( 'NONE',  ( 37.80618814713138676, -17.70384086642190979, 69.62690120949091011 ) ) ;
#15748 = CARTESIAN_POINT ( 'NONE',  ( 38.31606138205700063, 5.594015759443068170, 2.006005027196319901 ) ) ;
#15749 = VECTOR ( 'NONE', #3822, 1000.000000000000000 ) ;
#15750 = CARTESIAN_POINT ( 'NONE',  ( 39.95015449827720744, -12.61368208888610454, 70.79240656858105751 ) ) ;
#15751 = ORIENTED_EDGE ( 'NONE', *, *, #22713, .F. ) ;
#15752 = CARTESIAN_POINT ( 'NONE',  ( 36.98690846071097837, -23.81368208888611093, 73.30173637941817333 ) ) ;
#15753 = VERTEX_POINT ( 'NONE', #24106 ) ;
#15754 = CARTESIAN_POINT ( 'NONE',  ( 44.81606138205700063, 36.92314894770293421, 79.37823623207323465 ) ) ;
#15755 = CARTESIAN_POINT ( 'NONE',  ( 40.31606138205701484, -19.24645833192448308, 25.04281637636312041 ) ) ;
#15756 = CARTESIAN_POINT ( 'NONE',  ( 38.63098279924290068, -24.70384086642190979, 72.53360434286901182 ) ) ;
#15757 = ORIENTED_EDGE ( 'NONE', *, *, #1235, .F. ) ;
#15758 = ORIENTED_EDGE ( 'NONE', *, *, #23088, .F. ) ;
#15759 = FACE_OUTER_BOUND ( 'NONE', #274, .T. ) ;
#15760 = CARTESIAN_POINT ( 'NONE',  ( 36.31606138205700773, -18.80550481115971451, 25.27912300651437150 ) ) ;
#15762 = VECTOR ( 'NONE', #17445, 1000.000000000000227 ) ;
#15761 = DIRECTION ( 'NONE',  ( 0.000000000000000000, 3.469446951953613400E-15, 1.000000000000000000 ) ) ;
#15763 = CARTESIAN_POINT ( 'NONE',  ( 40.14115730948191185, -1.103840866421911260, 71.43714994484034264 ) ) ;
#15764 = VECTOR ( 'NONE', #3758, 1000.000000000000114 ) ;
#15765 = ADVANCED_FACE ( 'NONE', ( #18209 ), #18457, .F. ) ;
#15766 = FACE_OUTER_BOUND ( 'NONE', #8127, .T. ) ;
#15767 = CARTESIAN_POINT ( 'NONE',  ( 40.26954217208371034, -0.7136820888861000745, 69.89063713639259845 ) ) ;
#15768 = AXIS2_PLACEMENT_3D ( 'NONE', #10606, #6603, #15882 ) ;
#15769 = DIRECTION ( 'NONE',  ( 0.000000000000000000, -0.5706330172266920187, 0.8212051873014210024 ) ) ;
#15770 = ORIENTED_EDGE ( 'NONE', *, *, #13038, .T. ) ;
#15771 = ORIENTED_EDGE ( 'NONE', *, *, #19001, .T. ) ;
#15772 = DIRECTION ( 'NONE',  ( 4.336808689942074435E-17, -1.000000000000000000, 3.491481338843135327E-15 ) ) ;
#15773 = DIRECTION ( 'NONE',  ( 0.000000000000000000, 1.000000000000000000, 0.000000000000000000 ) ) ;
#15774 = CARTESIAN_POINT ( 'NONE',  ( 37.25202387243754032, -22.40384086642191619, 72.75271321436731853 ) ) ;
#15775 = DIRECTION ( 'NONE',  ( 0.000000000000000000, -1.000000000000000000, 2.775557561562891351E-15 ) ) ;
#15776 = ORIENTED_EDGE ( 'NONE', *, *, #10358, .T. ) ;
#15777 =( GEOMETRIC_REPRESENTATION_CONTEXT ( 3 ) GLOBAL_UNCERTAINTY_ASSIGNED_CONTEXT ( ( #20601 ) ) GLOBAL_UNIT_ASSIGNED_CONTEXT ( ( #21242, #25076, #11340 ) ) REPRESENTATION_CONTEXT ( 'NONE', 'WORKASPACE' ) );
#15778 = LINE ( 'NONE', #23753, #15979 ) ;
#15779 = AXIS2_PLACEMENT_3D ( 'NONE', #12652, #18438, #12902 ) ;
#15780 = CARTESIAN_POINT ( 'NONE',  ( 36.31606138205700063, -16.48551471403133206, 77.11349248448009064 ) ) ;
#15781 = EDGE_LOOP ( 'NONE', ( #4708, #15589, #11111, #17857 ) ) ;
#15782 = CARTESIAN_POINT ( 'NONE',  ( 37.25260217561390874, -8.003840866421910505, 70.97781676520604321 ) ) ;
#15783 = PLANE ( 'NONE',  #25368 ) ;
#15784 = EDGE_LOOP ( 'NONE', ( #10569, #12584, #6845, #20785 ) ) ;
#15785 = CARTESIAN_POINT ( 'NONE',  ( 30.81606138205706458, -34.55876147768187678, 70.30501292735635843 ) ) ;
#15786 = ORIENTED_EDGE ( 'NONE', *, *, #6026, .F. ) ;
#15787 = VERTEX_POINT ( 'NONE', #18711 ) ;
#15788 = CARTESIAN_POINT ( 'NONE',  ( 41.14099152588522657, 1.392818861812999964, 83.30501292736997243 ) ) ;
#15789 = CARTESIAN_POINT ( 'NONE',  ( 38.26194895904383486, -11.01368208888609956, 70.24448340153877268 ) ) ;
#15790 = CARTESIAN_POINT ( 'NONE',  ( 38.00113996487114321, -7.913682088886101695, 72.53360434286905445 ) ) ;
#15791 = VERTEX_POINT ( 'NONE', #6987 ) ;
#15792 = TOROIDAL_SURFACE ( 'NONE', #23530, 0.2314957320545545372, 0.5000000000000000000 ) ;
#15793 = ORIENTED_EDGE ( 'NONE', *, *, #24179, .F. ) ;
#15794 = DIRECTION ( 'NONE',  ( 1.000000000000000000, 0.000000000000000000, 0.000000000000000000 ) ) ;
#15795 = CARTESIAN_POINT ( 'NONE',  ( 33.32114655809477455, -33.12114953149414021, 59.73560708446382250 ) ) ;
#15796 = ORIENTED_EDGE ( 'NONE', *, *, #1119, .F. ) ;
#15797 = DIRECTION ( 'NONE',  ( 1.000000000000000000, 0.000000000000000000, 0.000000000000000000 ) ) ;
#15798 = CARTESIAN_POINT ( 'NONE',  ( 36.80608444377001831, -20.30384086642191477, 72.40698646996135324 ) ) ;
#15799 = EDGE_CURVE ( 'NONE', #22279, #22756, #1047, .T. ) ;
#15800 = EDGE_CURVE ( 'NONE', #12061, #3532, #22827, .T. ) ;
#15801 = DIRECTION ( 'NONE',  ( -1.000000000000000000, 1.040834085586084551E-30, 3.469446951953615175E-16 ) ) ;
#15802 = FACE_OUTER_BOUND ( 'NONE', #1162, .T. ) ;
#15803 = CARTESIAN_POINT ( 'NONE',  ( 38.37017380507020192, -16.01368208888609956, 72.51602215082118619 ) ) ;
#15804 = VERTEX_POINT ( 'NONE', #7114 ) ;
#15805 = ORIENTED_EDGE ( 'NONE', *, *, #7148, .T. ) ;
#15806 = CARTESIAN_POINT ( 'NONE',  ( 43.31606138205700063, 4.103895195095678794, 6.341006091748962348 ) ) ;
#15807 = CARTESIAN_POINT ( 'NONE',  ( 39.29254315202756231, -12.81368208888610383, 69.94417936956672577 ) ) ;
#15808 = CARTESIAN_POINT ( 'NONE',  ( 43.31606138205700773, -21.39087554181786643, 28.82307548518891238 ) ) ;
#15809 = DIRECTION ( 'NONE',  ( -1.000000000000000000, 1.115179377413661005E-30, 3.717264591378870232E-16 ) ) ;
#15810 = PLANE ( 'NONE',  #4093 ) ;
#15811 = LINE ( 'NONE', #21738, #5692 ) ;
#15812 = ADVANCED_FACE ( 'NONE', ( #22946 ), #8925, .F. ) ;
#15813 = DIRECTION ( 'NONE',  ( -1.000000000000000000, 0.000000000000000000, 0.000000000000000000 ) ) ;
#15814 = ORIENTED_EDGE ( 'NONE', *, *, #900, .T. ) ;
#15815 = AXIS2_PLACEMENT_3D ( 'NONE', #22202, #19635, #24489 ) ;
#15816 = B_SPLINE_CURVE_WITH_KNOTS ( 'NONE', 3,
 ( #6811, #24555, #6936, #20725 ),
 .UNSPECIFIED., .F., .F.,
 ( 4, 4 ),
 ( 0.000000000000000000, 1.000000000000000000 ),
 .UNSPECIFIED. ) ;
#15817 = CARTESIAN_POINT ( 'NONE',  ( 43.39709375099405975, 3.108381023609500193, 6.137326095127844994 ) ) ;
#15818 = ORIENTED_EDGE ( 'NONE', *, *, #19837, .T. ) ;
#15819 = EDGE_LOOP ( 'NONE', ( #22604, #1292 ) ) ;
#15820 = CARTESIAN_POINT ( 'NONE',  ( 38.26194895904384197, -6.603840866421920808, 73.71602215082116061 ) ) ;
#15821 = ORIENTED_EDGE ( 'NONE', *, *, #20081, .F. ) ;
#15822 = CARTESIAN_POINT ( 'NONE',  ( 33.31606138205700773, -12.76023008545321069, 21.53290024082827969 ) ) ;
#15823 = CARTESIAN_POINT ( 'NONE',  ( 37.80618814713140097, -7.913682088886107913, 73.13360434286904876 ) ) ;
#15824 = EDGE_LOOP ( 'NONE', ( #15520, #34, #13613, #13660, #12311, #5037 ) ) ;
#15825 = LINE ( 'NONE', #2162, #16147 ) ;
#15826 = CARTESIAN_POINT ( 'NONE',  ( 36.11133435605973574, -17.61368208888610454, 72.15350918040385864 ) ) ;
#15827 = FILL_AREA_STYLE ('',( #7860 ) ) ;
#15828 = CARTESIAN_POINT ( 'NONE',  ( 34.06606138205700773, -37.53049398575952722, 70.06662099985003067 ) ) ;
#15829 = DIRECTION ( 'NONE',  ( 0.000000000000000000, -1.000000000000000000, 3.469446951953613794E-15 ) ) ;
#15830 = SHAPE_REPRESENTATION_RELATIONSHIP ( 'NONE' , 'NONE' ,  #18165, #1241 ) ;
#15831 = CARTESIAN_POINT ( 'NONE',  ( 40.31606138205700773, -31.05876147765399864, 74.30501292737010033 ) ) ;
#15832 = EDGE_CURVE ( 'NONE', #20815, #5208, #6851, .T. ) ;
#15833 = PLANE ( 'NONE',  #964 ) ;
#15834 = CARTESIAN_POINT ( 'NONE',  ( 32.81606138205700773, -38.55876147765401640, 70.30501292737012875 ) ) ;
#15835 = CARTESIAN_POINT ( 'NONE',  ( 39.31564783533280405, -22.31368208888609672, 72.03616607671141026 ) ) ;
#15836 = ORIENTED_EDGE ( 'NONE', *, *, #5648, .T. ) ;
#15837 = CARTESIAN_POINT ( 'NONE',  ( 40.31606138205698642, -6.850818256144539653, 29.86554089437370152 ) ) ;
#15838 = DIRECTION ( 'NONE',  ( 0.000000000000000000, -0.5706330172266952383, 0.8212051873014186709 ) ) ;
#15839 = EDGE_LOOP ( 'NONE', ( #25425, #8288, #9533, #14378 ) ) ;
#15840 = ORIENTED_EDGE ( 'NONE', *, *, #5702, .T. ) ;
#15841 = CARTESIAN_POINT ( 'NONE',  ( 39.73277004305197124, -25.40384086642191264, 69.52238214136765748 ) ) ;
#15842 = CARTESIAN_POINT ( 'NONE',  ( 38.00113996487114321, -21.91368208888610170, 72.53360434286904024 ) ) ;
#15843 = CARTESIAN_POINT ( 'NONE',  ( 36.11133435605973574, -5.613682088886105426, 72.15350918040385864 ) ) ;
#15844 = ORIENTED_EDGE ( 'NONE', *, *, #6421, .T. ) ;
#15845 = DIRECTION ( 'NONE',  ( 9.925461516413219746E-16, -0.8967398287344630070, -0.4425581086832393041 ) ) ;
#15846 = CARTESIAN_POINT ( 'NONE',  ( 39.75915168707251723, -28.90384086642191619, 72.49904802271737481 ) ) ;
#15847 = ADVANCED_FACE ( 'NONE', ( #12797 ), #18967, .F. ) ;
#15848 = DIRECTION ( 'NONE',  ( -2.690219486203388234E-15, 0.8967398287344627850, 0.4425581086832399147 ) ) ;
#15849 = EDGE_CURVE ( 'NONE', #13664, #22879, #22694, .T. ) ;
#15850 = EDGE_LOOP ( 'NONE', ( #9744, #17185, #3539, #1419 ) ) ;
#15851 = PLANE ( 'NONE',  #9674 ) ;
#15852 = DIRECTION ( 'NONE',  ( 0.000000000000000000, 0.5706330172266907974, -0.8212051873014217795 ) ) ;
#15853 = CARTESIAN_POINT ( 'NONE',  ( 36.07789103942399578, -4.203840866421913347, 72.05058123536544201 ) ) ;
#15854 = EDGE_CURVE ( 'NONE', #21433, #13492, #15092, .T. ) ;
#15855 = EDGE_CURVE ( 'NONE', #5247, #23734, #18246, .T. ) ;
#15856 = EDGE_CURVE ( 'NONE', #24417, #25393, #10861, .T. ) ;
#15857 = DIRECTION ( 'NONE',  ( 0.000000000000000000, 3.469446951953613400E-15, 1.000000000000000000 ) ) ;
#15858 = CARTESIAN_POINT ( 'NONE',  ( 36.64852494920107517, -5.413682088886106136, 70.89533451361948835 ) ) ;
#15859 = CYLINDRICAL_SURFACE ( 'NONE', #9769, 3.000000000000000444 ) ;
#15860 = CARTESIAN_POINT ( 'NONE',  ( 39.82603832034401847, -24.31368208888611093, 72.40698646996131060 ) ) ;
#15861 = CARTESIAN_POINT ( 'NONE',  ( 33.31606138205700773, -10.66749763588700617, 14.47455635838400134 ) ) ;
#15862 = EDGE_CURVE ( 'NONE', #24921, #7305, #13043, .T. ) ;
#15863 = CARTESIAN_POINT ( 'NONE',  ( 39.29254315202757653, -4.803840866421913880, 72.81632618279323310 ) ) ;
#15865 = EDGE_CURVE ( 'NONE', #2738, #5929, #3369, .T. ) ;
#15864 = CONTEXT_DEPENDENT_SHAPE_REPRESENTATION ( #16207, #16095 ) ;
#15866 = CARTESIAN_POINT ( 'NONE',  ( 30.81606138205706813, -35.90867894478445521, 74.07034463014319670 ) ) ;
#15867 = CARTESIAN_POINT ( 'NONE',  ( 38.26194895904383486, -17.01368208888610312, 69.64448340153877837 ) ) ;
#15868 = FACE_OUTER_BOUND ( 'NONE', #9753, .T. ) ;
#15869 = CARTESIAN_POINT ( 'NONE',  ( 39.38009889167648936, -11.40384086642190908, 70.00779233799264034 ) ) ;
#15870 = DIRECTION ( 'NONE',  ( -1.734723475976804876E-16, 0.8212051873014210024, 0.5706330172266920187 ) ) ;
#15871 = EDGE_CURVE ( 'NONE', #16610, #21433, #18579, .T. ) ;
#15872 = CARTESIAN_POINT ( 'NONE',  ( 37.69796330110504101, -13.11368208888609743, 69.66206559358661821 ) ) ;
#15873 = VERTEX_POINT ( 'NONE', #2976 ) ;
#15874 = CARTESIAN_POINT ( 'NONE',  ( 39.12911128074873801, -20.11368208888610809, 73.69843995877327814 ) ) ;
#15875 = ORIENTED_EDGE ( 'NONE', *, *, #8487, .T. ) ;
#15876 = LINE ( 'NONE', #4668, #11936 ) ;
#15877 = CARTESIAN_POINT ( 'NONE',  ( 30.81606138205694378, 5.290470704224592424, -0.3848988112044732235 ) ) ;
#15878 = CARTESIAN_POINT ( 'NONE',  ( 39.31564783533279694, -15.30384086642191477, 70.72433947564853440 ) ) ;
#15879 = ORIENTED_EDGE ( 'NONE', *, *, #16250, .T. ) ;
#15880 = ORIENTED_EDGE ( 'NONE', *, *, #20761, .T. ) ;
#15881 = CARTESIAN_POINT ( 'NONE',  ( 39.63090472924900354, -28.94648940971289264, 70.80759201118661395 ) ) ;
#15882 = DIRECTION ( 'NONE',  ( 0.000000000000000000, -1.000000000000000000, 6.938893903907222067E-15 ) ) ;
#15883 = CARTESIAN_POINT ( 'NONE',  ( 36.29569395875881099, -20.30384086642191122, 72.77780686321128201 ) ) ;
#15884 = DIRECTION ( 'NONE',  ( 0.000000000000000000, 0.000000000000000000, -1.000000000000000000 ) ) ;
#15885 = CARTESIAN_POINT ( 'NONE',  ( 39.64521430340304420, -0.8136820888860993861, 69.45876917294177133 ) ) ;
#15886 = PRODUCT_DEFINITION_SHAPE ( 'NONE', 'NONE',  #2830 ) ;
#15887 = CARTESIAN_POINT ( 'NONE',  ( 44.81606138205700063, 44.92314894770293421, 79.37823623207320622 ) ) ;
#15888 = VERTEX_POINT ( 'NONE', #16646 ) ;
#15889 = ORIENTED_EDGE ( 'NONE', *, *, #13000, .F. ) ;
#15890 = FACE_OUTER_BOUND ( 'NONE', #23606, .T. ) ;
#15891 = FACE_OUTER_BOUND ( 'NONE', #23513, .T. ) ;
#15892 = EDGE_CURVE ( 'NONE', #12198, #14019, #21138, .T. ) ;
#15893 = CARTESIAN_POINT ( 'NONE',  ( 36.64852494920107517, -24.20384086642190979, 71.86517103874047052 ) ) ;
#15894 = SURFACE_SIDE_STYLE ('',( #12304 ) ) ;
#15895 = LINE ( 'NONE', #7930, #21920 ) ;
#15896 = EDGE_LOOP ( 'NONE', ( #6957, #24995, #6814, #8035 ) ) ;
#15897 = LINE ( 'NONE', #21582, #10675 ) ;
#15898 = DIRECTION ( 'NONE',  ( -1.000000000000000000, -3.091505625455828697E-15, -4.515976121274772923E-17 ) ) ;
#15899 = VERTEX_POINT ( 'NONE', #24867 ) ;
#15900 = CARTESIAN_POINT ( 'NONE',  ( 37.12184278917507640, -6.103840866421912814, 71.32335560751961623 ) ) ;
#15901 = DIRECTION ( 'NONE',  ( 1.734723475976814737E-16, -1.000000000000000000, 3.491481338843135327E-15 ) ) ;
#15902 = ORIENTED_EDGE ( 'NONE', *, *, #7602, .F. ) ;
#15903 = EDGE_CURVE ( 'NONE', #7024, #19403, #5052, .T. ) ;
#15904 = CARTESIAN_POINT ( 'NONE',  ( 43.81606138205700063, -22.55876147765401996, 68.80501292737008612 ) ) ;
#15905 = ORIENTED_EDGE ( 'NONE', *, *, #1072, .F. ) ;
#15906 = ORIENTED_EDGE ( 'NONE', *, *, #22249, .F. ) ;
#15907 = CARTESIAN_POINT ( 'NONE',  ( 38.31606138205700063, 42.51966564709218233, 71.30501292737018559 ) ) ;
#15908 = CARTESIAN_POINT ( 'NONE',  ( 39.37952058850012804, -6.613682088886101873, 70.97781676520601479 ) ) ;
#15909 = CARTESIAN_POINT ( 'NONE',  ( 39.37952058850012804, -2.613682088886102761, 70.97781676520601479 ) ) ;
#15910 = EDGE_LOOP ( 'NONE', ( #21152, #18243, #12947, #22119 ) ) ;
#15911 = ORIENTED_EDGE ( 'NONE', *, *, #25288, .T. ) ;
#15912 = CARTESIAN_POINT ( 'NONE',  ( 38.31606138205700773, -21.82678658219787948, 29.70634659473178019 ) ) ;
#15913 = LINE ( 'NONE', #10007, #3387 ) ;
#15914 = ORIENTED_EDGE ( 'NONE', *, *, #6723, .F. ) ;
#15915 = LINE ( 'NONE', #12074, #9945 ) ;
#15916 = CARTESIAN_POINT ( 'NONE',  ( 39.29254315202757653, -14.80384086642191477, 72.81632618279321889 ) ) ;
#15917 = VECTOR ( 'NONE', #18186, 1000.000000000000000 ) ;
#15918 = CIRCLE ( 'NONE', #22503, 1.499999999999999778 ) ;
#15919 = CARTESIAN_POINT ( 'NONE',  ( 38.05466885408097255, -22.20915446671475735, 75.80998910758448517 ) ) ;
#15920 = CARTESIAN_POINT ( 'NONE',  ( 31.81606138205700418, -34.67340937580780036, 71.26505871168839690 ) ) ;
#15921 = DIRECTION ( 'NONE',  ( 3.965082230804126670E-15, -0.8967398287344626739, -0.4425581086832401922 ) ) ;
#15922 = ORIENTED_EDGE ( 'NONE', *, *, #1840, .F. ) ;
#15923 = ORIENTED_EDGE ( 'NONE', *, *, #21150, .F. ) ;
#15924 = CARTESIAN_POINT ( 'NONE',  ( 44.31606138205700063, -20.93319939328399926, 43.78741072286599945 ) ) ;
#15925 = CARTESIAN_POINT ( 'NONE',  ( 39.75915168707250302, -16.71368208888609885, 70.26145752964252722 ) ) ;
#15926 = DIRECTION ( 'NONE',  ( -1.000000000000000000, 0.000000000000000000, 0.000000000000000000 ) ) ;
#15927 = CARTESIAN_POINT ( 'NONE',  ( 44.81606138205700063, -34.55876147765400219, 75.30501292737011454 ) ) ;
#15928 = CYLINDRICAL_SURFACE ( 'NONE', #18485, 12.59999999999999964 ) ;
#15929 = DIRECTION ( 'NONE',  ( 9.925461516413219746E-16, -0.8967398287344630070, -0.4425581086832393041 ) ) ;
#15930 = EDGE_CURVE ( 'NONE', #11231, #24067, #24815, .T. ) ;
#15931 = PLANE ( 'NONE',  #18095 ) ;
#15932 = CARTESIAN_POINT ( 'NONE',  ( 43.31606138205700063, 7.282926244446933595, 65.60596383066929604 ) ) ;
#15933 = EDGE_CURVE ( 'NONE', #20004, #23532, #3847, .T. ) ;
#15934 = CIRCLE ( 'NONE', #8124, 4.000000000000000000 ) ;
#15935 = AXIS2_PLACEMENT_3D ( 'NONE', #7701, #15545, #23394 ) ;
#15936 = EDGE_CURVE ( 'NONE', #12560, #24557, #20899, .T. ) ;
#15937 = PLANE ( 'NONE',  #20602 ) ;
#15938 = VERTEX_POINT ( 'NONE', #16511 ) ;
#15939 = ORIENTED_EDGE ( 'NONE', *, *, #3446, .F. ) ;
#15940 = CARTESIAN_POINT ( 'NONE',  ( 36.07789103942399578, -4.203840866421913347, 72.05058123536544201 ) ) ;
#15941 = ORIENTED_EDGE ( 'NONE', *, *, #7856, .T. ) ;
#15942 = PLANE ( 'NONE',  #21484 ) ;
#15943 = CARTESIAN_POINT ( 'NONE',  ( 37.33957961208646736, -9.813682088886107380, 72.81632618279323310 ) ) ;
#15944 = ORIENTED_EDGE ( 'NONE', *, *, #8938, .T. ) ;
#15945 = LINE ( 'NONE', #4113, #7116 ) ;
#15946 = ADVANCED_FACE ( 'NONE', ( #9566 ), #11623, .T. ) ;
#15947 = CARTESIAN_POINT ( 'NONE',  ( 36.98690846071097837, -13.81368208888610916, 73.30173637941818754 ) ) ;
#15948 = VECTOR ( 'NONE', #23950, 1000.000000000000227 ) ;
#15949 = DIRECTION ( 'NONE',  ( 0.000000000000000000, 0.6568589528324747517, -0.7540134720837718962 ) ) ;
#15950 = VECTOR ( 'NONE', #18063, 1000.000000000000114 ) ;
#15951 = CARTESIAN_POINT ( 'NONE',  ( 32.81606138205700063, 3.939336499464421770, 6.271597994279004773 ) ) ;
#15952 = PLANE ( 'NONE',  #16545 ) ;
#15953 = CARTESIAN_POINT ( 'NONE',  ( 36.31606138205700063, 37.94123852234599781, 75.30501292736988717 ) ) ;
#15954 = CYLINDRICAL_SURFACE ( 'NONE', #8808, 0.5000000000000004441 ) ;
#15955 = CARTESIAN_POINT ( 'NONE',  ( 33.31606138205700773, 10.62769494289597993, 68.29765714199933768 ) ) ;
#15956 = CARTESIAN_POINT ( 'NONE',  ( 37.31647492878122563, -25.31368208888610027, 70.72433947564853440 ) ) ;
#15957 = ORIENTED_EDGE ( 'NONE', *, *, #717, .T. ) ;
#15958 = CARTESIAN_POINT ( 'NONE',  ( 38.83707137437546919, -22.15992917496056691, 75.81017972364469415 ) ) ;
#15959 = CARTESIAN_POINT ( 'NONE',  ( 32.81606138205700773, -37.34243788671330577, 70.80615726751818784 ) ) ;
#15960 = ORIENTED_EDGE ( 'NONE', *, *, #4479, .F. ) ;
#15961 = AXIS2_PLACEMENT_3D ( 'NONE', #22876, #5233, #24413 ) ;
#15962 = EDGE_LOOP ( 'NONE', ( #17736, #10561, #18565, #17830 ) ) ;
#15963 = CARTESIAN_POINT ( 'NONE',  ( 40.52078840805429394, -23.00384086642191761, 72.15350918040381600 ) ) ;
#15964 = VECTOR ( 'NONE', #23147, 1000.000000000000114 ) ;
#15965 = CARTESIAN_POINT ( 'NONE',  ( 39.95015449827720744, -28.61368208888610454, 70.79240656858104330 ) ) ;
#15966 = FACE_OUTER_BOUND ( 'NONE', #2843, .T. ) ;
#15967 = ADVANCED_BREP_SHAPE_REPRESENTATION ( '', ( #16726, #2000 ), #15777 ) ;
#15968 = LINE ( 'NONE', #2562, #19244 ) ;
#15969 = VERTEX_POINT ( 'NONE', #17287 ) ;
#15970 = LINE ( 'NONE', #2192, #22428 ) ;
#15971 = DIRECTION ( 'NONE',  ( 1.734723475976804876E-16, 3.491481338843135327E-15, 1.000000000000000000 ) ) ;
#15972 = EDGE_CURVE ( 'NONE', #16502, #10392, #12909, .T. ) ;
#15973 = CARTESIAN_POINT ( 'NONE',  ( 37.61123632939164452, -5.703840866421911571, 69.02690120949094421 ) ) ;
#15974 = DIRECTION ( 'NONE',  ( 1.734723475976814737E-16, -1.000000000000000000, 3.491481338843135327E-15 ) ) ;
#15975 = CARTESIAN_POINT ( 'NONE',  ( 39.75915168707250302, -10.71368208888609885, 70.26145752964252722 ) ) ;
#15976 = LINE ( 'NONE', #2446, #15430 ) ;
#15977 = CARTESIAN_POINT ( 'NONE',  ( 39.75915168707250302, -26.71368208888609885, 70.26145752964251301 ) ) ;
#15978 = STYLED_ITEM ( 'NONE', ( #15187 ), #8266 ) ;
#15979 = VECTOR ( 'NONE', #21828, 1000.000000000000000 ) ;
#15980 = CARTESIAN_POINT ( 'NONE',  ( 30.81606138205697931, -4.589472609077253296, -6.350807634294811876 ) ) ;
#15981 = CARTESIAN_POINT ( 'NONE',  ( 39.75915168707251723, -0.9038408664219163002, 72.49904802271740323 ) ) ;
#15982 = ITEM_DEFINED_TRANSFORMATION ( 'NONE', 'NONE', #3471,  #2000 ) ;
#15983 = DIRECTION ( 'NONE',  ( 1.000000000000000000, 0.000000000000000000, 0.000000000000000000 ) ) ;
#15984 = ADVANCED_FACE ( 'NONE', ( #7754 ), #1804, .T. ) ;
#15985 = AXIS2_PLACEMENT_3D ( 'NONE', #5031, #3213, #12901 ) ;
#15986 = CARTESIAN_POINT ( 'NONE',  ( 39.41296390513587511, -27.20384086642191690, 71.08074471024438878 ) ) ;
#15987 = CARTESIAN_POINT ( 'NONE',  ( 37.25202387243752611, -9.213682088886100630, 70.00779233799264034 ) ) ;
#15988 = ADVANCED_FACE ( 'NONE', ( #15596 ), #5434, .T. ) ;
#15989 = CARTESIAN_POINT ( 'NONE',  ( 33.66606138205693810, 6.105630034208183510, 5.871938670042847974 ) ) ;
#15990 = CIRCLE ( 'NONE', #3653, 0.7500000000000031086 ) ;
#15991 = CARTESIAN_POINT ( 'NONE',  ( 39.82603832034400426, -13.30384086642190233, 70.35351908239857721 ) ) ;
#15992 = ADVANCED_FACE ( 'NONE', ( #1549 ), #5946, .T. ) ;
#15993 = CARTESIAN_POINT ( 'NONE',  ( 33.31606138205700773, -16.77230293220685198, 77.52306850662458260 ) ) ;
#15994 = CARTESIAN_POINT ( 'NONE',  ( 36.68196826583682935, -13.61368208888610454, 71.96809898377888715 ) ) ;
#15995 = EDGE_LOOP ( 'NONE', ( #15176, #12795, #10038, #23761 ) ) ;
#15996 = CARTESIAN_POINT ( 'NONE',  ( 39.12911128074873801, -16.11368208888610809, 73.69843995877327814 ) ) ;
#15997 = ORIENTED_EDGE ( 'NONE', *, *, #16488, .F. ) ;
#15998 = LINE ( 'NONE', #23849, #14815 ) ;
#15999 = DIRECTION ( 'NONE',  ( 1.000000000000000000, 0.000000000000000000, 0.000000000000000000 ) ) ;
#16000 = CARTESIAN_POINT ( 'NONE',  ( 37.38336156205273397, -17.90384086642190908, 70.63227792289247020 ) ) ;
#16001 = CIRCLE ( 'NONE', #784, 0.9023161253044892360 ) ;
#16002 = EDGE_LOOP ( 'NONE', ( #13963, #18665, #4838, #20241 ) ) ;
#16003 = ORIENTED_EDGE ( 'NONE', *, *, #19763, .F. ) ;
#16004 = CARTESIAN_POINT ( 'NONE',  ( 28.81606138205697576, -29.47337283097074945, 44.07055847651731995 ) ) ;
#16005 = CARTESIAN_POINT ( 'NONE',  ( 30.81606138205709300, -43.53621639303160862, 70.30601027268440362 ) ) ;
#16006 = EDGE_CURVE ( 'NONE', #21390, #15554, #17546, .T. ) ;
#16007 = CARTESIAN_POINT ( 'NONE',  ( 36.36258059203030513, -25.90384086642191264, 69.89063713639258424 ) ) ;
#16008 = AXIS2_PLACEMENT_3D ( 'NONE', #1780, #13275, #21127 ) ;
#16009 = DIRECTION ( 'NONE',  ( 1.734723475976805122E-16, 3.491481338843134933E-15, 1.000000000000000000 ) ) ;
#16010 = CARTESIAN_POINT ( 'NONE',  ( 36.49096545463212493, -25.51368208888609956, 71.43714994484030001 ) ) ;
#16011 = CARTESIAN_POINT ( 'NONE',  ( 32.81606138205700773, 44.92314894770294131, 81.17823623207320338 ) ) ;
#16012 = ORIENTED_EDGE ( 'NONE', *, *, #19494, .T. ) ;
#16013 = VECTOR ( 'NONE', #595, 1000.000000000000000 ) ;
#16014 = EDGE_LOOP ( 'NONE', ( #15939, #3613, #617, #3515, #7479, #1347, #22505 ) ) ;
#16015 = DIRECTION ( 'NONE',  ( 0.000000000000000000, -1.000000000000000000, 4.625929269271485322E-15 ) ) ;
#16016 = LINE ( 'NONE', #14472, #18013 ) ;
#16017 = CARTESIAN_POINT ( 'NONE',  ( 37.80618814713138676, -21.70384086642190979, 69.62690120949091011 ) ) ;
#16018 = CARTESIAN_POINT ( 'NONE',  ( 45.81606138205707168, -36.80651332587431313, 65.82119181171029254 ) ) ;
#16019 = ADVANCED_FACE ( 'NONE', ( #21402 ), #5564, .F. ) ;
#16020 = VECTOR ( 'NONE', #16725, 1000.000000000000227 ) ;
#16021 = VERTEX_POINT ( 'NONE', #13423 ) ;
#16022 = EDGE_CURVE ( 'NONE', #20938, #18511, #21124, .T. ) ;
#16023 = DIRECTION ( 'NONE',  ( -1.000000000000000000, 5.204170427930415223E-30, 1.734723475976805122E-15 ) ) ;
#16024 = EDGE_CURVE ( 'NONE', #1658, #2590, #13800, .T. ) ;
#16025 = CARTESIAN_POINT ( 'NONE',  ( 33.31606138205700773, -33.60910547091194900, 60.61426200347987248 ) ) ;
#16026 = ADVANCED_FACE ( 'NONE', ( #21533 ), #15346, .T. ) ;
#16027 = CARTESIAN_POINT ( 'NONE',  ( 38.93987200065210175, -2.803840866421911660, 72.33091598616827866 ) ) ;
#16028 = EDGE_CURVE ( 'NONE', #9377, #9429, #1672, .T. ) ;
#16029 = DIRECTION ( 'NONE',  ( 9.925461516413219746E-16, -0.8967398287344630070, -0.4425581086832393041 ) ) ;
#16030 = ORIENTED_EDGE ( 'NONE', *, *, #17559, .T. ) ;
#16031 = CARTESIAN_POINT ( 'NONE',  ( 38.26194895904383486, -29.01368208888610312, 69.64448340153876416 ) ) ;
#16032 = EDGE_LOOP ( 'NONE', ( #3599, #23662 ) ) ;
#16033 = ORIENTED_EDGE ( 'NONE', *, *, #16814, .T. ) ;
#16034 = DIRECTION ( 'NONE',  ( -1.000000000000000000, 0.000000000000000000, 0.000000000000000000 ) ) ;
#16035 = LINE ( 'NONE', #8445, #4298 ) ;
#16036 = VECTOR ( 'NONE', #15898, 1000.000000000000000 ) ;
#16037 = CARTESIAN_POINT ( 'NONE',  ( 37.89291511884476904, -7.113682088886103649, 70.26206559358664094 ) ) ;
#16038 = CARTESIAN_POINT ( 'NONE',  ( 38.73920764526925353, -6.113682088886101873, 72.49843995877331793 ) ) ;
#16039 = VERTEX_POINT ( 'NONE', #3881 ) ;
#16040 = ORIENTED_EDGE ( 'NONE', *, *, #14782, .T. ) ;
#16041 = CARTESIAN_POINT ( 'NONE',  ( 43.81606138205700063, -37.34243788671330577, 70.80615726751818784 ) ) ;
#16042 = FACE_OUTER_BOUND ( 'NONE', #19231, .T. ) ;
#16043 = VERTEX_POINT ( 'NONE', #25246 ) ;
#16044 = EDGE_CURVE ( 'NONE', #3140, #17954, #19464, .T. ) ;
#16045 = FACE_OUTER_BOUND ( 'NONE', #4293, .T. ) ;
#16046 = VECTOR ( 'NONE', #8017, 1000.000000000000114 ) ;
#16047 = CARTESIAN_POINT ( 'NONE',  ( 39.29254315202757653, -10.80384086642191477, 72.81632618279323310 ) ) ;
#16048 = CARTESIAN_POINT ( 'NONE',  ( 37.66883992158368955, -22.12338502244167060, 75.81039767295206389 ) ) ;
#16049 = DIRECTION ( 'NONE',  ( 1.000000000000000000, 2.999999999999999839E-15, -5.603103565922875308E-33 ) ) ;
#16050 = EDGE_LOOP ( 'NONE', ( #568, #14627, #9799, #23259 ) ) ;
#16051 = EDGE_LOOP ( 'NONE', ( #6510, #21581, #18364, #4319 ) ) ;
#16052 = CARTESIAN_POINT ( 'NONE',  ( 43.31606138205700063, -20.88462213363798270, 44.49284693533410717 ) ) ;
#16053 = AXIS2_PLACEMENT_3D ( 'NONE', #11493, #19333, #17280 ) ;
#16054 = CARTESIAN_POINT ( 'NONE',  ( 39.29254315202756231, -6.813682088886101162, 69.94417936956673998 ) ) ;
#16055 = ADVANCED_FACE ( 'NONE', ( #21154 ), #7629, .T. ) ;
#16056 = CARTESIAN_POINT ( 'NONE',  ( 32.81606138205700773, -33.60910547091194900, 60.61426200347987248 ) ) ;
#16057 = FACE_OUTER_BOUND ( 'NONE', #22057, .T. ) ;
#16058 = VECTOR ( 'NONE', #18270, 1000.000000000000000 ) ;
#16059 = DIRECTION ( 'NONE',  ( 0.000000000000000000, -3.225463739888140187E-15, -1.000000000000000000 ) ) ;
#16060 = FACE_OUTER_BOUND ( 'NONE', #5369, .T. ) ;
#16061 = CARTESIAN_POINT ( 'NONE',  ( 43.31606138205700063, -21.31259689655800216, 45.10875082581016926 ) ) ;
#16062 = CARTESIAN_POINT ( 'NONE',  ( 43.81606138205700063, 44.92314894770294131, 80.37823623207322044 ) ) ;
#16063 = ORIENTED_EDGE ( 'NONE', *, *, #20498, .F. ) ;
#16064 = CARTESIAN_POINT ( 'NONE',  ( 32.81606138205700773, 35.38401127291550097, 61.48364296169660292 ) ) ;
#16065 = ORIENTED_EDGE ( 'NONE', *, *, #17309, .T. ) ;
#16066 = ORIENTED_EDGE ( 'NONE', *, *, #15903, .F. ) ;
#16067 = DIRECTION ( 'NONE',  ( 0.000000000000000000, 1.000000000000000000, -3.469446951953613400E-15 ) ) ;
#16068 = CARTESIAN_POINT ( 'NONE',  ( 37.61123632939164452, -1.703840866421911571, 69.02690120949094421 ) ) ;
#16069 = CIRCLE ( 'NONE', #24694, 9.500000000000000000 ) ;
#16070 = ORIENTED_EDGE ( 'NONE', *, *, #15365, .T. ) ;
#16071 = FACE_OUTER_BOUND ( 'NONE', #1154, .T. ) ;
#16072 = CARTESIAN_POINT ( 'NONE',  ( 39.38009889167650357, -6.213682088886108623, 72.75271321436733274 ) ) ;
#16073 = AXIS2_PLACEMENT_3D ( 'NONE', #13473, #13234, #1726 ) ;
#16074 = ORIENTED_EDGE ( 'NONE', *, *, #4100, .T. ) ;
#16075 = DIRECTION ( 'NONE',  ( 1.327674326049719602E-15, -0.4425581086832399147, 0.8967398287344627850 ) ) ;
#16076 = CARTESIAN_POINT ( 'NONE',  ( 39.64521430340304420, -16.81368208888610383, 69.45876917294175712 ) ) ;
#16077 = EDGE_CURVE ( 'NONE', #18272, #15541, #10025, .T. ) ;
#16078 = PLANE ( 'NONE',  #1157 ) ;
#16079 = EDGE_CURVE ( 'NONE', #7819, #16874, #21654, .T. ) ;
#16080 = DIRECTION ( 'NONE',  ( -1.445602896647339903E-16, 1.000000000000000000, -2.999999999999999839E-15 ) ) ;
#16081 = DIRECTION ( 'NONE',  ( 0.000000000000000000, 0.000000000000000000, 1.000000000000000000 ) ) ;
#16082 = SURFACE_STYLE_FILL_AREA ( #10297 ) ;
#16083 = LINE ( 'NONE', #4250, #12320 ) ;
#16084 = DIRECTION ( 'NONE',  ( 1.327674326049719602E-15, -0.4425581086832399147, 0.8967398287344627850 ) ) ;
#16085 = AXIS2_PLACEMENT_3D ( 'NONE', #17490, #17106, #25315 ) ;
#16086 = CARTESIAN_POINT ( 'NONE',  ( 33.40064408022072939, 42.38065457974295924, 79.52109337493037344 ) ) ;
#16087 = CARTESIAN_POINT ( 'NONE',  ( 37.12184278917507640, -25.51368208888609956, 71.43714994484032843 ) ) ;
#16088 = ORIENTED_EDGE ( 'NONE', *, *, #5157, .T. ) ;
#16089 = CARTESIAN_POINT ( 'NONE',  ( 39.32240756636089429, -21.96791893307624832, 75.80813956697402034 ) ) ;
#16090 = EDGE_CURVE ( 'NONE', #5182, #20407, #9319, .T. ) ;
#16091 = DIRECTION ( 'NONE',  ( 1.000000000000000000, 2.490066548941357423E-15, 1.228895056384528013E-15 ) ) ;
#16092 = ORIENTED_EDGE ( 'NONE', *, *, #3804, .T. ) ;
#16093 = ORIENTED_EDGE ( 'NONE', *, *, #13412, .F. ) ;
#16094 = CARTESIAN_POINT ( 'NONE',  ( 36.89935272106205133, -26.40384086642191974, 73.23812341099225875 ) ) ;
#16095 = PRODUCT_DEFINITION_SHAPE ( 'NONE', 'NONE',  #25494 ) ;
#16096 = CARTESIAN_POINT ( 'NONE',  ( 36.80608444377001121, -27.31368208888610383, 70.35351908239857721 ) ) ;
#16097 = DIRECTION ( 'NONE',  ( 0.000000000000000000, 1.000000000000000000, -2.921639538487253867E-15 ) ) ;
#16098 = ORIENTED_EDGE ( 'NONE', *, *, #22406, .T. ) ;
#16099 = DIRECTION ( 'NONE',  ( 1.000000000000000000, 0.000000000000000000, 0.000000000000000000 ) ) ;
#16100 = DIRECTION ( 'NONE',  ( 1.000000000000000000, 0.000000000000000000, 0.000000000000000000 ) ) ;
#16101 = CARTESIAN_POINT ( 'NONE',  ( 38.26194895904384197, -0.6038408664219181432, 73.71602215082116061 ) ) ;
#16102 = EDGE_CURVE ( 'NONE', #5023, #25151, #17859, .T. ) ;
#16103 = DIRECTION ( 'NONE',  ( 0.000000000000000000, 1.163336342344335610E-15, -1.000000000000000000 ) ) ;
#16105 = EDGE_CURVE ( 'NONE', #22104, #5709, #9625, .T. ) ;
#16104 = FACE_OUTER_BOUND ( 'NONE', #18600, .T. ) ;
#16106 = CARTESIAN_POINT ( 'NONE',  ( 38.93415946300897446, -6.113682088886107202, 73.09843995877331224 ) ) ;
#16107 = CARTESIAN_POINT ( 'NONE',  ( 36.31606138205700063, 8.691238522346997897, 68.80501292736998664 ) ) ;
#16108 = PRESENTATION_LAYER_ASSIGNMENT (  '', '', ( #12018 ) ) ;
#16109 = CARTESIAN_POINT ( 'NONE',  ( 38.93415946300898867, -28.11368208888610454, 73.09843995877328382 ) ) ;
#16110 = CARTESIAN_POINT ( 'NONE',  ( 36.31606138205700773, -19.47805968271055477, 24.94720442500192448 ) ) ;
#16111 = CARTESIAN_POINT ( 'NONE',  ( 40.64099152588523367, 1.392818861812999964, 93.30501292736998664 ) ) ;
#16112 = DIRECTION ( 'NONE',  ( -1.000000000000000000, -1.187136597504755470E-16, -8.249087426255173666E-17 ) ) ;
#16113 = CARTESIAN_POINT ( 'NONE',  ( 39.31564783533279694, -27.30384086642191477, 70.72433947564850598 ) ) ;
#16114 = CARTESIAN_POINT ( 'NONE',  ( 39.38009889167650357, -14.21368208888610773, 72.75271321436731853 ) ) ;
#16115 = LINE ( 'NONE', #23969, #23014 ) ;
#16116 = EDGE_CURVE ( 'NONE', #13605, #22410, #10844, .T. ) ;
#16117 = VECTOR ( 'NONE', #21340, 1000.000000000000000 ) ;
#16118 = VECTOR ( 'NONE', #19818, 1000.000000000000000 ) ;
#16119 = CARTESIAN_POINT ( 'NONE',  ( 39.82603832034400426, -9.303840866421907663, 70.35351908239857721 ) ) ;
#16120 = CARTESIAN_POINT ( 'NONE',  ( 38.31606138205687273, 42.19123852234595518, 61.30501292736988006 ) ) ;
#16121 = VECTOR ( 'NONE', #2902, 1000.000000000000000 ) ;
#16122 = CARTESIAN_POINT ( 'NONE',  ( 36.87297107704152666, -13.71368208888610773, 72.49904802271740323 ) ) ;
#16123 = ORIENTED_EDGE ( 'NONE', *, *, #15441, .T. ) ;
#16124 = CARTESIAN_POINT ( 'NONE',  ( 39.12911128074873801, -18.11368208888610454, 73.69843995877327814 ) ) ;
#16125 = VERTEX_POINT ( 'NONE', #2566 ) ;
#16126 = DIRECTION ( 'NONE',  ( 0.000000000000000000, 3.129456975819164530E-15, 1.000000000000000000 ) ) ;
#16127 = DIRECTION ( 'NONE',  ( 1.000000000000000000, 0.000000000000000000, 0.000000000000000000 ) ) ;
#16128 = CARTESIAN_POINT ( 'NONE',  ( 39.41296390513587511, -21.20384086642190979, 71.08074471024441721 ) ) ;
#16129 = ORIENTED_EDGE ( 'NONE', *, *, #10182, .T. ) ;
#16130 = ORIENTED_EDGE ( 'NONE', *, *, #6786, .F. ) ;
#16131 = DIRECTION ( 'NONE',  ( -2.690219486203388234E-15, 0.8967398287344627850, 0.4425581086832399147 ) ) ;
#16132 = CARTESIAN_POINT ( 'NONE',  ( 43.31606138205700063, -10.19550266980812658, 14.63954348514304904 ) ) ;
#16133 = CARTESIAN_POINT ( 'NONE',  ( 38.26194895904384197, -24.60384086642191903, 73.71602215082113219 ) ) ;
#16134 = LINE ( 'NONE', #8293, #989 ) ;
#16135 = CARTESIAN_POINT ( 'NONE',  ( 40.14115730948191185, -28.51368208888610667, 71.32335560751958781 ) ) ;
#16136 = DIRECTION ( 'NONE',  ( 1.000000000000000000, 3.001186103030333510E-15, 2.281710121244060993E-16 ) ) ;
#16137 = VECTOR ( 'NONE', #18782, 1000.000000000000114 ) ;
#16138 = EDGE_LOOP ( 'NONE', ( #9718, #17448 ) ) ;
#16139 = CARTESIAN_POINT ( 'NONE',  ( 43.81606138205700063, -27.11289203277224402, 56.96090842897168471 ) ) ;
#16140 = DIRECTION ( 'NONE',  ( -1.327674326049719602E-15, 0.4425581086832399147, -0.8967398287344627850 ) ) ;
#16141 = AXIS2_PLACEMENT_3D ( 'NONE', #17074, #20808, #22475 ) ;
#16142 = CARTESIAN_POINT ( 'NONE',  ( 40.14115730948191185, -23.10384086642191548, 71.43714994484031422 ) ) ;
#16143 =( NAMED_UNIT ( * ) PLANE_ANGLE_UNIT ( ) SI_UNIT ( $, .RADIAN. ) );
#16144 = FACE_OUTER_BOUND ( 'NONE', #17573, .T. ) ;
#16145 = CARTESIAN_POINT ( 'NONE',  ( 44.81606138205700063, -38.55876147765410167, 70.30501292737011454 ) ) ;
#16146 = CIRCLE ( 'NONE', #24781, 1.100000000000000311 ) ;
#16147 = VECTOR ( 'NONE', #10417, 1000.000000000000000 ) ;
#16148 = CARTESIAN_POINT ( 'NONE',  ( 40.71606138205694947, 3.586515973360791421, -0.5067327973472466329 ) ) ;
#16149 = CARTESIAN_POINT ( 'NONE',  ( 37.21915885897815457, -2.203840866421911571, 71.67976084211552745 ) ) ;
#16150 = DIRECTION ( 'NONE',  ( 0.000000000000000000, -0.3299742535181005021, 0.9439899321577387425 ) ) ;
#16151 = VERTEX_POINT ( 'NONE', #8129 ) ;
#16152 = DIRECTION ( 'NONE',  ( 1.000000000000000000, 0.000000000000000000, 0.000000000000000000 ) ) ;
#16153 = EDGE_LOOP ( 'NONE', ( #25069, #15002, #18860, #15386 ) ) ;
#16154 = VERTEX_POINT ( 'NONE', #2311 ) ;
#16155 = DIRECTION ( 'NONE',  ( -1.000000000000000000, -2.999999999999999839E-15, 0.000000000000000000 ) ) ;
#16156 = AXIS2_PLACEMENT_3D ( 'NONE', #14509, #14759, #12717 ) ;
#16157 = LINE ( 'NONE', #24009, #922 ) ;
#16158 = UNCERTAINTY_MEASURE_WITH_UNIT (LENGTH_MEASURE( 1.000000000000000082E-05 ), #25249, 'distance_accuracy_value', 'NONE');
#16159 = CARTESIAN_POINT ( 'NONE',  ( 37.69225076346193504, -3.813682088886102051, 72.33091598616827866 ) ) ;
#16160 = CARTESIAN_POINT ( 'NONE',  ( 39.41296390513587511, -6.413682088886100807, 71.67976084211552745 ) ) ;
#16161 = ORIENTED_EDGE ( 'NONE', *, *, #15865, .T. ) ;
#16162 = VERTEX_POINT ( 'NONE', #2064 ) ;
#16163 = CARTESIAN_POINT ( 'NONE',  ( 45.81606138205696510, -29.47337283097071037, 44.07055847651734837 ) ) ;
#16164 = AXIS2_PLACEMENT_3D ( 'NONE', #2845, #1306, #4792 ) ;
#16165 = CARTESIAN_POINT ( 'NONE',  ( 44.06606138205700063, 40.39281886181299797, 82.55501292736983032 ) ) ;
#16166 = LINE ( 'NONE', #6394, #24307 ) ;
#16167 = CARTESIAN_POINT ( 'NONE',  ( 38.82593461698265003, -12.70384086642191512, 73.13360434286903455 ) ) ;
#16168 = EDGE_CURVE ( 'NONE', #18026, #13623, #21785, .T. ) ;
#16169 = CARTESIAN_POINT ( 'NONE',  ( 36.31606138205700063, 39.69123852234597649, 69.30501292736988717 ) ) ;
#16170 = EDGE_CURVE ( 'NONE', #24865, #17786, #14188, .T. ) ;
#16171 = CARTESIAN_POINT ( 'NONE',  ( 36.41626118072728246, -20.92866386383740718, 75.89769837076177339 ) ) ;
#16172 = AXIS2_PLACEMENT_3D ( 'NONE', #16851, #4745, #12863 ) ;
#16173 = CYLINDRICAL_SURFACE ( 'NONE', #6864, 0.7500000000000027756 ) ;
#16174 = ADVANCED_FACE ( 'NONE', ( #4519 ), #4144, .F. ) ;
#16175 = ORIENTED_EDGE ( 'NONE', *, *, #4282, .F. ) ;
#16176 = EDGE_LOOP ( 'NONE', ( #4476, #23569, #13005, #14084 ) ) ;
#16177 = EDGE_CURVE ( 'NONE', #16934, #7904, #13313, .T. ) ;
#16178 = EDGE_CURVE ( 'NONE', #23726, #3683, #10440, .T. ) ;
#16179 = ORIENTED_EDGE ( 'NONE', *, *, #14762, .F. ) ;
#16180 = CARTESIAN_POINT ( 'NONE',  ( 45.81606138205705747, -32.32696853385078128, 75.83798663122490780 ) ) ;
#16181 = CARTESIAN_POINT ( 'NONE',  ( 36.80608444377001121, -9.313682088886100274, 70.35351908239861984 ) ) ;
#16182 = DIRECTION ( 'NONE',  ( -1.000000000000000000, 5.204170427930415223E-30, 1.734723475976805122E-15 ) ) ;
#16183 = VECTOR ( 'NONE', #8272, 1000.000000000000000 ) ;
#16184 = LINE ( 'NONE', #14383, #5446 ) ;
#16185 = CARTESIAN_POINT ( 'NONE',  ( 43.81606138205700063, -36.55876147765400930, 73.30501292737011454 ) ) ;
#16186 = CARTESIAN_POINT ( 'NONE',  ( 46.81606138205707168, -35.90867894478441258, 74.07034463014319670 ) ) ;
#16187 = VECTOR ( 'NONE', #21028, 1000.000000000000000 ) ;
#16188 = ADVANCED_FACE ( 'NONE', ( #21907 ), #248, .F. ) ;
#16189 = ADVANCED_FACE ( 'NONE', ( #20101 ), #6569, .F. ) ;
#16190 = DIRECTION ( 'NONE',  ( 0.000000000000000000, -0.3299742535180970049, 0.9439899321577400748 ) ) ;
#16191 = PLANE ( 'NONE',  #15141 ) ;
#16192 = CARTESIAN_POINT ( 'NONE',  ( 44.81606138205700063, 36.92314894770293421, 80.37823623207323465 ) ) ;
#16193 = ORIENTED_EDGE ( 'NONE', *, *, #22216, .T. ) ;
#16194 = ORIENTED_EDGE ( 'NONE', *, *, #24899, .T. ) ;
#16195 = CARTESIAN_POINT ( 'NONE',  ( 43.31606138205700063, -4.357181138186127178, 82.80501292736992980 ) ) ;
#16196 = CARTESIAN_POINT ( 'NONE',  ( 40.55423172469004101, -3.203840866421916456, 70.70992431699450265 ) ) ;
#16197 = ORIENTED_EDGE ( 'NONE', *, *, #23406, .T. ) ;
#16198 = CARTESIAN_POINT ( 'NONE',  ( 40.31606138205700773, 43.19123852234599781, 74.30501292736987295 ) ) ;
#16199 = CARTESIAN_POINT ( 'NONE',  ( 36.80608444377001121, -9.313682088886100274, 70.35351908239860563 ) ) ;
#16200 = CIRCLE ( 'NONE', #5108, 3.000000000000002665 ) ;
#16201 = FACE_BOUND ( 'NONE', #3202, .T. ) ;
#16202 = CIRCLE ( 'NONE', #5113, 1.750000000000001998 ) ;
#16203 = CARTESIAN_POINT ( 'NONE',  ( 40.77203464402485622, -16.51368208888610667, 71.32335560751960202 ) ) ;
#16204 = CARTESIAN_POINT ( 'NONE',  ( 38.31606138205700063, -0.7263636227174442572, 61.39059882987834982 ) ) ;
#16205 = FACE_OUTER_BOUND ( 'NONE', #11746, .T. ) ;
#16206 = DIRECTION ( 'NONE',  ( 1.000000000000000000, -3.982629455510873500E-31, -4.336808689942015271E-16 ) ) ;
#16208 = FILL_AREA_STYLE_COLOUR ( '', #17873 ) ;
#16207 =( REPRESENTATION_RELATIONSHIP ('NONE','NONE', #17377, #15514 ) REPRESENTATION_RELATIONSHIP_WITH_TRANSFORMATION ( #18064 )SHAPE_REPRESENTATION_RELATIONSHIP( ) );
#16209 = STYLED_ITEM ( 'NONE', ( #15450 ), #1241 ) ;
#16210 = DIRECTION ( 'NONE',  ( 0.000000000000000000, 0.6568589528324746407, -0.7540134720837717852 ) ) ;
#16211 = VECTOR ( 'NONE', #13706, 1000.000000000000000 ) ;
#16212 = VECTOR ( 'NONE', #24363, 1000.000000000000000 ) ;
#16213 = CARTESIAN_POINT ( 'NONE',  ( 33.40064408022072939, 40.76768529863396395, 79.57823623207325170 ) ) ;
#16214 = DIRECTION ( 'NONE',  ( 1.000000000000000000, 0.000000000000000000, 0.000000000000000000 ) ) ;
#16215 = CARTESIAN_POINT ( 'NONE',  ( 39.31564783533280405, -24.31368208888610383, 72.03616607671136762 ) ) ;
#16216 = ORIENTED_EDGE ( 'NONE', *, *, #10186, .T. ) ;
#16217 = DIRECTION ( 'NONE',  ( -0.000000000000000000, -1.000000000000000000, 2.999999999999998655E-15 ) ) ;
#16218 = COLOUR_RGB ( '', 0.72549020, 0.75294118, 0.79215686) ;
#16219 = CARTESIAN_POINT ( 'NONE',  ( 33.31606138205700773, 7.187001342539796944, 66.09667597968754649 ) ) ;
#16220 = ORIENTED_EDGE ( 'NONE', *, *, #19959, .F. ) ;
#16221 = EDGE_LOOP ( 'NONE', ( #3923, #3733, #4327, #1759 ) ) ;
#16222 = PRODUCT_DEFINITION_CONTEXT ( 'detailed design', #6029, 'design' ) ;
#16223 = CARTESIAN_POINT ( 'NONE',  ( 40.77203464402485622, -21.10384086642191548, 71.43714994484032843 ) ) ;
#16224 = ADVANCED_FACE ( 'NONE', ( #4271 ), #374, .F. ) ;
#16225 = CARTESIAN_POINT ( 'NONE',  ( 37.50301148336529167, 0.8863179111139005695, 69.06206559358666652 ) ) ;
#16226 = ADVANCED_FACE ( 'NONE', ( #4395 ), #23705, .T. ) ;
#16227 = DIRECTION ( 'NONE',  ( 0.000000000000000000, 2.999999999999999839E-15, 1.000000000000000000 ) ) ;
#16228 = ORIENTED_EDGE ( 'NONE', *, *, #22533, .F. ) ;
#16229 = AXIS2_PLACEMENT_3D ( 'NONE', #6999, #6865, #20398 ) ;
#16230 = PLANE ( 'NONE',  #25403 ) ;
#16231 = FILL_AREA_STYLE ('',( #17574 ) ) ;
#16232 = VERTEX_POINT ( 'NONE', #18310 ) ;
#16233 = CARTESIAN_POINT ( 'NONE',  ( 43.31606138205700063, -38.37466412126273951, 70.68129701848354784 ) ) ;
#16234 = CARTESIAN_POINT ( 'NONE',  ( 42.99361969242278292, 2.839052459004266726, 6.102834979010582472 ) ) ;
#16235 = CARTESIAN_POINT ( 'NONE',  ( 39.64521430340305841, -6.803840866421918321, 73.30173637941818754 ) ) ;
#16236 = FACE_OUTER_BOUND ( 'NONE', #16688, .T. ) ;
#16237 = DIRECTION ( 'NONE',  ( 0.000000000000000000, -3.469446951953611033E-15, -1.000000000000000000 ) ) ;
#16238 = CARTESIAN_POINT ( 'NONE',  ( 36.87297107704152666, -5.713682088886105959, 72.49904802271743165 ) ) ;
#16239 = CARTESIAN_POINT ( 'NONE',  ( 36.31606138205700063, 8.691238522346989015, 65.80501292736998664 ) ) ;
#16240 = CARTESIAN_POINT ( 'NONE',  ( 37.33957961208646736, -27.81368208888611093, 72.81632618279320468 ) ) ;
#16241 = DIRECTION ( 'NONE',  ( 1.000000000000000000, 1.156482317317870344E-15, 0.000000000000000000 ) ) ;
#16242 = DIRECTION ( 'NONE',  ( -2.122643018205887308E-17, 1.000000000000000000, -3.120611096041553009E-15 ) ) ;
#16243 = CARTESIAN_POINT ( 'NONE',  ( 39.24876120206129571, -22.90384086642191264, 72.12822762946747446 ) ) ;
#16244 = CARTESIAN_POINT ( 'NONE',  ( 39.95015449827720744, -12.61368208888610454, 70.79240656858105751 ) ) ;
#16245 = FACE_OUTER_BOUND ( 'NONE', #13699, .T. ) ;
#16246 = AXIS2_PLACEMENT_3D ( 'NONE', #9026, #19062, #22912 ) ;
#16247 = EDGE_CURVE ( 'NONE', #17440, #25304, #14307, .T. ) ;
#16248 = CARTESIAN_POINT ( 'NONE',  ( 38.37017380507018771, -9.603840866421908373, 69.64448340153879258 ) ) ;
#16249 = CARTESIAN_POINT ( 'NONE',  ( 45.81606138205700063, 40.39281886181299797, 80.75501292736983316 ) ) ;
#16250 = EDGE_CURVE ( 'NONE', #3936, #8692, #11882, .T. ) ;
#16251 = CARTESIAN_POINT ( 'NONE',  ( 38.26194895904383486, -13.01368208888610134, 69.64448340153877837 ) ) ;
#16252 = ORIENTED_EDGE ( 'NONE', *, *, #24831, .F. ) ;
#16253 = CARTESIAN_POINT ( 'NONE',  ( 36.29569395875879678, -15.31368208888610205, 69.98269868914867686 ) ) ;
#16254 = EDGE_LOOP ( 'NONE', ( #4825, #14742, #7455, #18262 ) ) ;
#16255 = CARTESIAN_POINT ( 'NONE',  ( 44.31606138205700063, 10.29926546647973851, 68.67466387804121553 ) ) ;
#16256 = CARTESIAN_POINT ( 'NONE',  ( 41.31606138205700063, 8.104266321858618838, 55.82104096753806033 ) ) ;
#16257 = CARTESIAN_POINT ( 'NONE',  ( 37.25260217561390874, -16.00384086642191050, 70.97781676520601479 ) ) ;
#16258 = ORIENTED_EDGE ( 'NONE', *, *, #19326, .F. ) ;
#16259 = VERTEX_POINT ( 'NONE', #16234 ) ;
#16260 = DIRECTION ( 'NONE',  ( -1.000000000000000000, 1.011922027653136605E-30, 3.373073425510455500E-16 ) ) ;
#16261 = LINE ( 'NONE', #4173, #10824 ) ;
#16262 = CARTESIAN_POINT ( 'NONE',  ( 39.64521430340305841, -24.80384086642191832, 73.30173637941817333 ) ) ;
#16263 = CARTESIAN_POINT ( 'NONE',  ( 30.81606138205705747, -33.21365173458017495, 70.96885009038120984 ) ) ;
#16264 = CARTESIAN_POINT ( 'NONE',  ( 37.69796330110504101, -25.11368208888609388, 69.66206559358660400 ) ) ;
#16265 = EDGE_CURVE ( 'NONE', #6560, #17850, #22154, .T. ) ;
#16266 = LINE ( 'NONE', #10229, #3606 ) ;
#16267 = VERTEX_POINT ( 'NONE', #6071 ) ;
#16268 = ORIENTED_EDGE ( 'NONE', *, *, #10967, .T. ) ;
#16269 = LINE ( 'NONE', #20650, #23171 ) ;
#16270 = DIRECTION ( 'NONE',  ( 1.000000000000000000, 0.000000000000000000, 0.000000000000000000 ) ) ;
#16271 = CARTESIAN_POINT ( 'NONE',  ( 39.29254315202757653, -16.80384086642191477, 72.81632618279321889 ) ) ;
#16272 = LINE ( 'NONE', #23870, #9998 ) ;
#16273 = CARTESIAN_POINT ( 'NONE',  ( 34.06606138205700773, 2.740850673309605412, 6.112030963703427133 ) ) ;
#16274 = LINE ( 'NONE', #2618, #19754 ) ;
#16275 = CARTESIAN_POINT ( 'NONE',  ( 38.63098279924290068, -2.703840866421912015, 72.53360434286905445 ) ) ;
#16276 = CARTESIAN_POINT ( 'NONE',  ( 40.31606138205700773, 37.44123852234599781, 74.30501292736988717 ) ) ;
#16277 = EDGE_LOOP ( 'NONE', ( #11182, #21194, #2740, #3943 ) ) ;
#16278 = DIRECTION ( 'NONE',  ( 1.000000000000000000, 2.999999999999999839E-15, 0.000000000000000000 ) ) ;
#16279 = ORIENTED_EDGE ( 'NONE', *, *, #23733, .F. ) ;
#16280 = ORIENTED_EDGE ( 'NONE', *, *, #22996, .F. ) ;
#16281 = CARTESIAN_POINT ( 'NONE',  ( 44.81606138205700063, 35.44123852234597649, 68.30501292736990138 ) ) ;
#16282 = DIRECTION ( 'NONE',  ( -4.625929269271484533E-15, 0.8967398287344634511, 0.4425581086832385824 ) ) ;
#16283 = CARTESIAN_POINT ( 'NONE',  ( 38.93987200065208754, -6.813682088886101162, 70.42958956619168021 ) ) ;
#16284 = CARTESIAN_POINT ( 'NONE',  ( 37.21915885897815457, -5.413682088886103472, 71.08074471024443142 ) ) ;
#16285 = ORIENTED_EDGE ( 'NONE', *, *, #22486, .F. ) ;
#16286 = ORIENTED_EDGE ( 'NONE', *, *, #15832, .T. ) ;
#16287 = CARTESIAN_POINT ( 'NONE',  ( 32.81606138205700773, -33.60910547091194900, 60.61426200347987248 ) ) ;
#16288 = LINE ( 'NONE', #24136, #12478 ) ;
#16289 = ORIENTED_EDGE ( 'NONE', *, *, #15127, .F. ) ;
#16290 = DIRECTION ( 'NONE',  ( 0.000000000000000000, -0.8212051873014203363, -0.5706330172266926848 ) ) ;
#16291 = CARTESIAN_POINT ( 'NONE',  ( 38.26194895904384907, -12.60384086642191548, 73.11602215082116629 ) ) ;
#16292 = CARTESIAN_POINT ( 'NONE',  ( 44.06606138205700063, 43.35512946304240245, 83.12823623207320622 ) ) ;
#16293 = ADVANCED_FACE ( 'NONE', ( #20358 ), #14807, .F. ) ;
#16294 = CARTESIAN_POINT ( 'NONE',  ( 38.31606138205700063, 38.19123852234599781, 71.30501292737001506 ) ) ;
#16295 = ORIENTED_EDGE ( 'NONE', *, *, #18172, .F. ) ;
#16296 = VERTEX_POINT ( 'NONE', #18678 ) ;
#16297 = CARTESIAN_POINT ( 'NONE',  ( 44.81606138205700063, 38.19123852234599070, 72.05501292736988717 ) ) ;
#16298 = CARTESIAN_POINT ( 'NONE',  ( 38.37017380507020192, -6.013682088886109334, 73.11602215082118050 ) ) ;
#16299 = CARTESIAN_POINT ( 'NONE',  ( 39.86921189136248955, -29.10876147765123179, 71.15716630587182578 ) ) ;
#16300 = DIRECTION ( 'NONE',  ( -2.690219486203388234E-15, 0.8967398287344627850, 0.4425581086832399147 ) ) ;
#16301 = FACE_OUTER_BOUND ( 'NONE', #941, .T. ) ;
#16302 = CARTESIAN_POINT ( 'NONE',  ( 36.31606138205702194, -19.24645833192449373, 25.04281637636312041 ) ) ;
#16303 = CARTESIAN_POINT ( 'NONE',  ( 40.31606138205702194, -21.82181003913286332, 31.95585308007613179 ) ) ;
#16304 = EDGE_CURVE ( 'NONE', #12100, #25424, #22769, .T. ) ;
#16305 = EDGE_CURVE ( 'NONE', #1848, #8440, #11282, .T. ) ;
#16306 = CARTESIAN_POINT ( 'NONE',  ( 41.31606138205700063, 7.043113989679085307, 66.83274420321491505 ) ) ;
#16307 = ORIENTED_EDGE ( 'NONE', *, *, #18776, .T. ) ;
#16308 = EDGE_CURVE ( 'NONE', #1085, #22152, #145, .T. ) ;
#16309 = ORIENTED_EDGE ( 'NONE', *, *, #12407, .T. ) ;
#16310 = CARTESIAN_POINT ( 'NONE',  ( 36.06606138205696510, -1.522470315718732037, 0.9921758631592225708 ) ) ;
#16311 = CARTESIAN_POINT ( 'NONE',  ( 38.26194895904383486, -27.01368208888609956, 69.04448340153878405 ) ) ;
#16312 = EDGE_CURVE ( 'NONE', #546, #14366, #11081, .T. ) ;
#16313 = AXIS2_PLACEMENT_3D ( 'NONE', #11922, #19380, #17463 ) ;
#16314 = CARTESIAN_POINT ( 'NONE',  ( 38.26194895904383486, -21.01368208888610312, 70.24448340153875847 ) ) ;
#16315 = ORIENTED_EDGE ( 'NONE', *, *, #8820, .F. ) ;
#16316 = ORIENTED_EDGE ( 'NONE', *, *, #15561, .F. ) ;
#16317 = LINE ( 'NONE', #20200, #4206 ) ;
#16318 = CARTESIAN_POINT ( 'NONE',  ( 39.75915168707250302, -6.713682088886099741, 70.26145752964252722 ) ) ;
#16319 = CARTESIAN_POINT ( 'NONE',  ( 37.12184278917507640, -2.103840866421912370, 71.32335560751961623 ) ) ;
#16320 = FACE_OUTER_BOUND ( 'NONE', #9904, .T. ) ;
#16321 = ADVANCED_FACE ( 'NONE', ( #6955 ), #14554, .T. ) ;
#16322 = CARTESIAN_POINT ( 'NONE',  ( 40.26954217208371034, -6.713682088886101518, 69.89063713639259845 ) ) ;
#16323 = LINE ( 'NONE', #10042, #15613 ) ;
#16324 = DIRECTION ( 'NONE',  ( 0.000000000000000000, 1.000000000000000000, -2.999999999999999839E-15 ) ) ;
#16325 = AXIS2_PLACEMENT_3D ( 'NONE', #23075, #17168, #6991 ) ;
#16326 = CIRCLE ( 'NONE', #21670, 0.5000000000000004441 ) ;
#16327 = LINE ( 'NONE', #4623, #23947 ) ;
#16328 = AXIS2_PLACEMENT_3D ( 'NONE', #1591, #17329, #25154 ) ;
#16329 = VECTOR ( 'NONE', #16667, 1000.000000000000000 ) ;
#16330 = DIRECTION ( 'NONE',  ( -2.122643018205885151E-17, 1.000000000000000000, -3.120611096041553009E-15 ) ) ;
#16331 = DIRECTION ( 'NONE',  ( 0.000000000000000000, 0.5706330172266920187, -0.8212051873014210024 ) ) ;
#16332 = VERTEX_POINT ( 'NONE', #7079 ) ;
#16333 = CARTESIAN_POINT ( 'NONE',  ( 39.82744760895728575, -21.53778768028494994, 75.32795621999423474 ) ) ;
#16334 = FACE_OUTER_BOUND ( 'NONE', #16153, .T. ) ;
#16335 = VERTEX_POINT ( 'NONE', #22412 ) ;
#16336 = VERTEX_POINT ( 'NONE', #18552 ) ;
#16337 = CARTESIAN_POINT ( 'NONE',  ( 37.50301148336529877, -20.50384086642191761, 73.69843995877327814 ) ) ;
#16338 = ADVANCED_FACE ( 'NONE', ( #24322 ), #876, .F. ) ;
#16339 = EDGE_CURVE ( 'NONE', #17824, #4130, #18800, .T. ) ;
#16340 = CARTESIAN_POINT ( 'NONE',  ( 38.37017380507020192, -26.01368208888611022, 73.11602215082115208 ) ) ;
#16341 = DIRECTION ( 'NONE',  ( 0.000000000000000000, 3.469446951953611033E-15, 1.000000000000000000 ) ) ;
#16342 = AXIS2_PLACEMENT_3D ( 'NONE', #20896, #10730, #20385 ) ;
#16343 = VECTOR ( 'NONE', #13186, 1000.000000000000000 ) ;
#16344 = VECTOR ( 'NONE', #11576, 1000.000000000000000 ) ;
#16345 = FACE_OUTER_BOUND ( 'NONE', #12047, .T. ) ;
#16346 = PLANE ( 'NONE',  #4875 ) ;
#16347 = VERTEX_POINT ( 'NONE', #2815 ) ;
#16348 = CARTESIAN_POINT ( 'NONE',  ( 32.56606138205700773, -26.74044063519535186, 82.55501292737007191 ) ) ;
#16349 = CARTESIAN_POINT ( 'NONE',  ( 43.31606138205700063, 6.289375473607850431, 7.138843309009015314 ) ) ;
#16350 = EDGE_CURVE ( 'NONE', #24211, #20287, #8771, .T. ) ;
#16351 = CARTESIAN_POINT ( 'NONE',  ( 39.73277004305197124, -1.403840866421909972, 69.52238214136768590 ) ) ;
#16352 = DIRECTION ( 'NONE',  ( -1.734723475976804876E-16, -3.469446951953610245E-15, -1.000000000000000000 ) ) ;
#16353 = CARTESIAN_POINT ( 'NONE',  ( 33.23058527440272059, 3.113468987225112006, 6.136968036621317069 ) ) ;
#16354 = CARTESIAN_POINT ( 'NONE',  ( 36.49096545463212493, -7.513682088886102228, 71.43714994484035685 ) ) ;
#16355 = PLANE ( 'NONE',  #20792 ) ;
#16356 = CARTESIAN_POINT ( 'NONE',  ( 38.26194895904383486, -19.01368208888610312, 69.64448340153877837 ) ) ;
#16357 = CARTESIAN_POINT ( 'NONE',  ( 45.81606138205697221, -4.349482454670838827, -5.142398479549302515 ) ) ;
#16358 = ADVANCED_FACE ( 'NONE', ( #24452 ), #24707, .F. ) ;
#16359 = AXIS2_PLACEMENT_3D ( 'NONE', #23578, #13797, #19716 ) ;
#16360 = DIRECTION ( 'NONE',  ( 0.000000000000000000, 1.000000000000000000, -2.999999999999999839E-15 ) ) ;
#16361 = CARTESIAN_POINT ( 'NONE',  ( 39.51027997493896748, -23.10384086642191548, 71.43714994484032843 ) ) ;
#16362 = CARTESIAN_POINT ( 'NONE',  ( 36.80608444377001121, -11.31368208888609672, 70.35351908239857721 ) ) ;
#16363 = AXIS2_PLACEMENT_3D ( 'NONE', #9851, #15769, #3410 ) ;
#16364 = AXIS2_PLACEMENT_3D ( 'NONE', #17464, #19381, #3285 ) ;
#16365 = DIRECTION ( 'NONE',  ( -1.327674326049719602E-15, 0.4425581086832399147, -0.8967398287344627850 ) ) ;
#16366 = EDGE_LOOP ( 'NONE', ( #9370, #3911, #7859, #7723 ) ) ;
#16367 = CARTESIAN_POINT ( 'NONE',  ( 39.75915168707251723, -8.903840866421916189, 72.49904802271740323 ) ) ;
#16368 = CARTESIAN_POINT ( 'NONE',  ( 44.81606138205700063, 40.39281886181299797, 81.75501292736983316 ) ) ;
#16369 = CARTESIAN_POINT ( 'NONE',  ( 36.80608444377001121, -7.313682088886100274, 70.35351908239860563 ) ) ;
#16370 = ORIENTED_EDGE ( 'NONE', *, *, #13126, .T. ) ;
#16371 = CARTESIAN_POINT ( 'NONE',  ( 40.26954217208371034, -14.71368208888610241, 69.89063713639258424 ) ) ;
#16372 = ORIENTED_EDGE ( 'NONE', *, *, #3453, .T. ) ;
#16373 = DIRECTION ( 'NONE',  ( -2.690219486203388234E-15, 0.8967398287344627850, 0.4425581086832399147 ) ) ;
#16374 = DIRECTION ( 'NONE',  ( 1.000000000000000000, 3.091505625455828697E-15, 4.515976121274736561E-17 ) ) ;
#16375 = CARTESIAN_POINT ( 'NONE',  ( 37.60469502381300799, -18.40384086642190908, 72.26730301774234988 ) ) ;
#16376 = ORIENTED_EDGE ( 'NONE', *, *, #10317, .T. ) ;
#16377 = ORIENTED_EDGE ( 'NONE', *, *, #2541, .F. ) ;
#16378 = FACE_OUTER_BOUND ( 'NONE', #23258, .T. ) ;
#16379 = LINE ( 'NONE', #24228, #928 ) ;
#16380 = CARTESIAN_POINT ( 'NONE',  ( 39.64521430340305841, -20.80384086642191832, 73.30173637941818754 ) ) ;
#16381 = VECTOR ( 'NONE', #20434, 1000.000000000000000 ) ;
#16382 = DIRECTION ( 'NONE',  ( 0.000000000000000000, 1.000000000000000000, 0.000000000000000000 ) ) ;
#16383 = CARTESIAN_POINT ( 'NONE',  ( 38.26194895904383486, -29.01368208888610312, 69.64448340153876416 ) ) ;
#16384 = CARTESIAN_POINT ( 'NONE',  ( 32.56606138205700773, 40.39281886181299797, 83.30501292736984453 ) ) ;
#16385 = CARTESIAN_POINT ( 'NONE',  ( 38.31606138205700063, -22.22127907754186893, 75.30501292736998664 ) ) ;
#16386 = ADVANCED_FACE ( 'NONE', ( #8645 ), #20612, .T. ) ;
#16387 = AXIS2_PLACEMENT_3D ( 'NONE', #3979, #19190, #21370 ) ;
#16388 = AXIS2_PLACEMENT_3D ( 'NONE', #4373, #23933, #3986 ) ;
#16389 = VERTEX_POINT ( 'NONE', #16739 ) ;
#16390 = ADVANCED_FACE ( 'NONE', ( #24572 ), #6693, .F. ) ;
#16391 = FACE_OUTER_BOUND ( 'NONE', #12550, .T. ) ;
#16392 = CARTESIAN_POINT ( 'NONE',  ( 43.23147868389327897, 42.38065457974295924, 79.52109337493035923 ) ) ;
#16393 = CARTESIAN_POINT ( 'NONE',  ( 36.64852494920107517, -14.20384086642191157, 71.86517103874048473 ) ) ;
#16394 = APPLICATION_PROTOCOL_DEFINITION ( 'draft international standard', 'automotive_design', 1998, #23629 ) ;
#16395 = FACE_OUTER_BOUND ( 'NONE', #14862, .T. ) ;
#16396 = COLOUR_RGB ( '', 0.09019608, 0.27058824, 0.51372549) ;
#16397 = DIRECTION ( 'NONE',  ( 0.000000000000000000, 0.4425581086832394706, -0.8967398287344628960 ) ) ;
#16398 = CIRCLE ( 'NONE', #3661, 0.4999999999999982792 ) ;
#16399 = CARTESIAN_POINT ( 'NONE',  ( 33.31606138205700773, -22.22127907754187959, 75.30501292736998664 ) ) ;
#16400 = CARTESIAN_POINT ( 'NONE',  ( 38.82593461698265003, -28.70384086642190624, 73.13360434286902034 ) ) ;
#16401 = CARTESIAN_POINT ( 'NONE',  ( 38.05217264712879199, -5.216721506228226168, 82.80003502201218168 ) ) ;
#16402 = EDGE_LOOP ( 'NONE', ( #18576, #24295, #8832, #22944 ) ) ;
#16403 = AXIS2_PLACEMENT_3D ( 'NONE', #10876, #16789, #8694 ) ;
#16404 = EDGE_CURVE ( 'NONE', #2906, #16878, #3031, .T. ) ;
#16405 = CARTESIAN_POINT ( 'NONE',  ( 37.80618814713140097, -23.91368208888610880, 73.13360434286902034 ) ) ;
#16406 = VERTEX_POINT ( 'NONE', #9157 ) ;
#16407 = ORIENTED_EDGE ( 'NONE', *, *, #6116, .F. ) ;
#16408 = CARTESIAN_POINT ( 'NONE',  ( 30.81606138205697576, -4.349482454670884124, -5.142398479549302515 ) ) ;
#16409 = DIRECTION ( 'NONE',  ( 0.000000000000000000, -1.000000000000000000, 2.999999999999999839E-15 ) ) ;
#16410 = CARTESIAN_POINT ( 'NONE',  ( 38.63098279924288647, -2.913682088886100363, 70.22690120949091863 ) ) ;
#16411 = AXIS2_PLACEMENT_3D ( 'NONE', #22895, #5261, #15169 ) ;
#16412 = CARTESIAN_POINT ( 'NONE',  ( 38.37017380507020192, -6.013682088886104005, 72.51602215082118619 ) ) ;
#16413 = ORIENTED_EDGE ( 'NONE', *, *, #11318, .F. ) ;
#16414 = ORIENTED_EDGE ( 'NONE', *, *, #23591, .F. ) ;
#16415 = CARTESIAN_POINT ( 'NONE',  ( 33.31606138205700773, 3.996716213179724697, 6.311483552851885115 ) ) ;
#16416 = CARTESIAN_POINT ( 'NONE',  ( 36.31606138205700063, 8.691238522346997897, 68.80501292736998664 ) ) ;
#16417 = VERTEX_POINT ( 'NONE', #17004 ) ;
#16418 = SURFACE_STYLE_FILL_AREA ( #12457 ) ;
#16419 = CARTESIAN_POINT ( 'NONE',  ( 38.93415946300896024, -9.503840866421908729, 69.66206559358663242 ) ) ;
#16420 = VECTOR ( 'NONE', #3189, 1000.000000000000000 ) ;
#16421 = CARTESIAN_POINT ( 'NONE',  ( 36.31606138205700063, -31.05876147765399864, 74.30501292737010033 ) ) ;
#16422 = CARTESIAN_POINT ( 'NONE',  ( 30.81606138205698997, -7.197381196808482429, -3.552044091124089142 ) ) ;
#16423 = ORIENTED_EDGE ( 'NONE', *, *, #6072, .T. ) ;
#16424 = ORIENTED_EDGE ( 'NONE', *, *, #13287, .F. ) ;
#16425 = ORIENTED_EDGE ( 'NONE', *, *, #19494, .F. ) ;
#16426 = VECTOR ( 'NONE', #17685, 1000.000000000000000 ) ;
#16427 = DIRECTION ( 'NONE',  ( -1.000000000000000000, -2.999999999999999839E-15, 0.000000000000000000 ) ) ;
#16428 = CARTESIAN_POINT ( 'NONE',  ( 37.33957961208646736, -7.813682088886109156, 72.81632618279323310 ) ) ;
#16429 = LINE ( 'NONE', #24280, #18423 ) ;
#16430 = DIRECTION ( 'NONE',  ( 1.000000000000000000, -5.204170427930415223E-30, -1.734723475976805122E-15 ) ) ;
#16431 = VECTOR ( 'NONE', #13110, 1000.000000000000227 ) ;
#16432 = CARTESIAN_POINT ( 'NONE',  ( 32.81606138205700773, 38.19123852234599070, 73.05501292736988717 ) ) ;
#16433 = VECTOR ( 'NONE', #5607, 1000.000000000000000 ) ;
#16434 = CARTESIAN_POINT ( 'NONE',  ( 40.81606138205700063, 9.191238522346999673, 69.30501292736997243 ) ) ;
#16435 = DIRECTION ( 'NONE',  ( 0.000000000000000000, 3.469446951953613400E-15, 1.000000000000000000 ) ) ;
#16436 = EDGE_CURVE ( 'NONE', #2969, #20881, #24837, .T. ) ;
#16437 = AXIS2_PLACEMENT_3D ( 'NONE', #19853, #5686, #19341 ) ;
#16438 = PLANE ( 'NONE',  #22238 ) ;
#16439 = EDGE_LOOP ( 'NONE', ( #16566, #15960, #10947, #22268 ) ) ;
#16440 = VERTEX_POINT ( 'NONE', #4642 ) ;
#16441 = LINE ( 'NONE', #2403, #20248 ) ;
#16442 = CARTESIAN_POINT ( 'NONE',  ( 36.07789103942399578, -0.2038408664219136524, 72.05058123536544201 ) ) ;
#16443 = VECTOR ( 'NONE', #24695, 1000.000000000000000 ) ;
#16444 = CARTESIAN_POINT ( 'NONE',  ( 39.02742774030102879, -24.21368208888609885, 72.26730301774232146 ) ) ;
#16445 = ORIENTED_EDGE ( 'NONE', *, *, #22923, .F. ) ;
#16446 = ORIENTED_EDGE ( 'NONE', *, *, #14762, .T. ) ;
#16447 = DIRECTION ( 'NONE',  ( 1.000000000000000000, 1.734723475976804876E-16, -1.734723475976814737E-16 ) ) ;
#16448 = CARTESIAN_POINT ( 'NONE',  ( 38.82593461698262871, -4.913682088886100807, 69.62690120949091011 ) ) ;
#16449 = CARTESIAN_POINT ( 'NONE',  ( 36.80608444377001831, -28.30384086642191122, 72.40698646996133903 ) ) ;
#16450 = CIRCLE ( 'NONE', #17698, 2.000000000000001776 ) ;
#16451 = CARTESIAN_POINT ( 'NONE',  ( 38.31606138205694378, 3.409598742320820719, 3.426245460917042074 ) ) ;
#16452 = CARTESIAN_POINT ( 'NONE',  ( 36.98690846071097837, -9.813682088886107380, 73.30173637941818754 ) ) ;
#16453 = VECTOR ( 'NONE', #12308, 1000.000000000000000 ) ;
#16454 = DIRECTION ( 'NONE',  ( 1.000000000000000000, 0.000000000000000000, 0.000000000000000000 ) ) ;
#16455 = DIRECTION ( 'NONE',  ( 0.000000000000000000, 0.7540134720837717852, 0.6568589528324747517 ) ) ;
#16456 = VECTOR ( 'NONE', #633, 1000.000000000000114 ) ;
#16457 = LINE ( 'NONE', #3056, #2754 ) ;
#16458 = DIRECTION ( 'NONE',  ( -1.000000000000000000, 0.000000000000000000, 0.000000000000000000 ) ) ;
#16459 = CARTESIAN_POINT ( 'NONE',  ( 40.05520938202761982, -6.159673327590979852, 82.75478415414899303 ) ) ;
#16460 = DIRECTION ( 'NONE',  ( -6.938893903907229955E-15, 1.000000000000000000, -2.999999999999999839E-15 ) ) ;
#16461 = ORIENTED_EDGE ( 'NONE', *, *, #1239, .T. ) ;
#16462 = CARTESIAN_POINT ( 'NONE',  ( 38.31606138205700063, -7.415330352220093069, 56.88974067930232081 ) ) ;
#16463 = ADVANCED_FACE ( 'NONE', ( #12522 ), #7855, .F. ) ;
#16464 = DIRECTION ( 'NONE',  ( 0.000000000000000000, -0.5706330172266920187, 0.8212051873014210024 ) ) ;
#16465 = VERTEX_POINT ( 'NONE', #17643 ) ;
#16466 = ORIENTED_EDGE ( 'NONE', *, *, #16339, .T. ) ;
#16467 = VECTOR ( 'NONE', #10152, 1000.000000000000000 ) ;
#16468 = CARTESIAN_POINT ( 'NONE',  ( 38.26194895904384197, -18.60384086642191548, 73.71602215082113219 ) ) ;
#16469 = CARTESIAN_POINT ( 'NONE',  ( 37.80618814713140097, -23.91368208888610880, 73.13360434286902034 ) ) ;
#16470 = FACE_OUTER_BOUND ( 'NONE', #19647, .T. ) ;
#16471 = LINE ( 'NONE', #20608, #9386 ) ;
#16472 = DIRECTION ( 'NONE',  ( 1.000000000000000000, 2.999999999999999839E-15, 0.000000000000000000 ) ) ;
#16473 = ORIENTED_EDGE ( 'NONE', *, *, #3655, .T. ) ;
#16474 = CARTESIAN_POINT ( 'NONE',  ( 40.04430115328838724, -6.141487559858251899, 82.76153007216328206 ) ) ;
#16475 = CARTESIAN_POINT ( 'NONE',  ( -3.469446951953610245E-16, 35.92314894770294131, 80.37823623207323465 ) ) ;
#16476 = CARTESIAN_POINT ( 'NONE',  ( 39.12911128074873801, -28.11368208888610809, 73.69843995877326392 ) ) ;
#16477 = ORIENTED_EDGE ( 'NONE', *, *, #23212, .T. ) ;
#16478 = EDGE_CURVE ( 'NONE', #19565, #25152, #5406, .T. ) ;
#16479 = CARTESIAN_POINT ( 'NONE',  ( 40.31606138205700773, -11.18542543036241987, 17.47151328161626793 ) ) ;
#16480 = LINE ( 'NONE', #16612, #23934 ) ;
#16481 = CARTESIAN_POINT ( 'NONE',  ( 36.49096545463212493, -3.513682088886103116, 71.43714994484035685 ) ) ;
#16482 = CARTESIAN_POINT ( 'NONE',  ( 45.61606138205700489, 36.92314894770294131, 81.37823623207324886 ) ) ;
#16483 = EDGE_CURVE ( 'NONE', #15633, #14611, #12930, .T. ) ;
#16484 = AXIS2_PLACEMENT_3D ( 'NONE', #22662, #16734, #6821 ) ;
#16485 = CARTESIAN_POINT ( 'NONE',  ( 39.75915168707250302, -18.71368208888610241, 70.26145752964252722 ) ) ;
#16486 = ADVANCED_FACE ( 'NONE', ( #15314 ), #23419, .F. ) ;
#16487 = ADVANCED_FACE ( 'NONE', ( #1641 ), #21366, .T. ) ;
#16488 = EDGE_CURVE ( 'NONE', #22023, #15369, #16601, .T. ) ;
#16489 =( BOUNDED_CURVE ( )  B_SPLINE_CURVE ( 3, ( #12757, #6941, #19052, #15174 ),
 .UNSPECIFIED., .F., .T. ) 
 B_SPLINE_CURVE_WITH_KNOTS ( ( 4, 4 ),
 ( 0.000000000000000000, 1.570796326794895004 ),
 .UNSPECIFIED. ) 
 CURVE ( )  GEOMETRIC_REPRESENTATION_ITEM ( )  RATIONAL_B_SPLINE_CURVE ( ( 1.000000000000000000, 0.8047378541243649375, 0.8047378541243649375, 1.000000000000000000 ) ) 
 REPRESENTATION_ITEM ( '' )  );
#16490 = CARTESIAN_POINT ( 'NONE',  ( 43.31606138205700063, 0.9984178969752143251, 11.59873562314662010 ) ) ;
#16491 = CARTESIAN_POINT ( 'NONE',  ( 46.46042646344656646, 1.361611432489177265, -2.592146606185704805 ) ) ;
#16492 = CARTESIAN_POINT ( 'NONE',  ( 38.93987200065210175, -26.80384086642191122, 72.33091598616823603 ) ) ;
#16493 = CARTESIAN_POINT ( 'NONE',  ( 36.80608444377001121, -7.313682088886100274, 70.35351908239860563 ) ) ;
#16494 = DIRECTION ( 'NONE',  ( -1.734723475976804876E-16, 1.000000000000000000, 0.000000000000000000 ) ) ;
#16495 = ORIENTED_EDGE ( 'NONE', *, *, #23237, .F. ) ;
#16496 = EDGE_CURVE ( 'NONE', #7089, #126, #13142, .T. ) ;
#16497 = CARTESIAN_POINT ( 'NONE',  ( 36.49096545463212493, -8.103840866421908373, 71.32335560751963044 ) ) ;
#16498 = DIRECTION ( 'NONE',  ( 1.000000000000000000, -0.000000000000000000, 0.000000000000000000 ) ) ;
#16499 = CARTESIAN_POINT ( 'NONE',  ( 40.14115730948191185, -2.513682088886103116, 71.32335560751961623 ) ) ;
#16500 = VERTEX_POINT ( 'NONE', #17132 ) ;
#16501 = CARTESIAN_POINT ( 'NONE',  ( 40.33642880535524000, -14.31368208888610738, 72.77780686321126780 ) ) ;
#16502 = VERTEX_POINT ( 'NONE', #1406 ) ;
#16503 = LINE ( 'NONE', #909, #7848 ) ;
#16504 = CARTESIAN_POINT ( 'NONE',  ( 43.81606138205700063, 41.44123852234595518, 61.30501292736988006 ) ) ;
#16505 = STYLED_ITEM ( 'NONE', ( #12830 ), #25224 ) ;
#16506 = CARTESIAN_POINT ( 'NONE',  ( 37.60469502381300799, -10.40384086642191086, 72.26730301774236409 ) ) ;
#16507 = CARTESIAN_POINT ( 'NONE',  ( 43.23147868389327897, 41.67000142393845152, 79.52109337493035923 ) ) ;
#16508 = EDGE_CURVE ( 'NONE', #4334, #7071, #23162, .T. ) ;
#16509 = ORIENTED_EDGE ( 'NONE', *, *, #14126, .F. ) ;
#16510 = DIRECTION ( 'NONE',  ( -1.000000000000000000, 5.510910596163088391E-31, 1.836970198721029688E-16 ) ) ;
#16511 = CARTESIAN_POINT ( 'NONE',  ( 40.31606138205700773, -29.30876147765401640, 69.30501292737010033 ) ) ;
#16512 = STYLED_ITEM ( 'NONE', ( #3499 ), #17413 ) ;
#16513 = CARTESIAN_POINT ( 'NONE',  ( 39.73277004305197124, -17.40384086642191264, 69.52238214136768590 ) ) ;
#16514 = DIRECTION ( 'NONE',  ( -1.000000000000000000, 0.000000000000000000, 0.000000000000000000 ) ) ;
#16515 = CARTESIAN_POINT ( 'NONE',  ( 38.93415946300897446, -28.11368208888610098, 73.09843995877328382 ) ) ;
#16516 = CYLINDRICAL_SURFACE ( 'NONE', #12941, 2.500000000000002220 ) ;
#16517 = DIRECTION ( 'NONE',  ( -4.336808689942020201E-16, -2.999999999999999839E-15, -1.000000000000000000 ) ) ;
#16518 = VERTEX_POINT ( 'NONE', #1518 ) ;
#16519 = DIRECTION ( 'NONE',  ( 0.000000000000000000, -1.000000000000000000, 2.999999999999999839E-15 ) ) ;
#16520 = CARTESIAN_POINT ( 'NONE',  ( 39.81746892067405952, 41.67000142393845152, 79.37823623207322044 ) ) ;
#16521 = CARTESIAN_POINT ( 'NONE',  ( 38.37017380507018771, -17.60384086642190837, 69.64448340153877837 ) ) ;
#16522 = DIRECTION ( 'NONE',  ( 0.000000000000000000, 0.000000000000000000, 1.000000000000000000 ) ) ;
#16523 = VECTOR ( 'NONE', #10545, 1000.000000000000000 ) ;
#16524 = DIRECTION ( 'NONE',  ( 1.000000000000000000, 0.000000000000000000, 0.000000000000000000 ) ) ;
#16525 = DIRECTION ( 'NONE',  ( 0.000000000000000000, -0.3299742535180969494, 0.9439899321577399638 ) ) ;
#16526 = AXIS2_PLACEMENT_3D ( 'NONE', #3209, #1019, #24711 ) ;
#16527 = CARTESIAN_POINT ( 'NONE',  ( 40.31606138205700773, -19.47805968271054766, 24.94720442500192448 ) ) ;
#16528 = CARTESIAN_POINT ( 'NONE',  ( 37.25260217561390874, -0.003840866421911393481, 70.97781676520604321 ) ) ;
#16529 = CARTESIAN_POINT ( 'NONE',  ( 37.09309150775561648, -5.596477263455031270, 82.79255245176237565 ) ) ;
#16530 = ORIENTED_EDGE ( 'NONE', *, *, #21999, .T. ) ;
#16531 = CARTESIAN_POINT ( 'NONE',  ( 36.80608444377001121, -25.31368208888610383, 70.35351908239857721 ) ) ;
#16532 = ORIENTED_EDGE ( 'NONE', *, *, #13756, .F. ) ;
#16533 = ORIENTED_EDGE ( 'NONE', *, *, #9081, .F. ) ;
#16534 = DIRECTION ( 'NONE',  ( 0.000000000000000000, -0.6568589528324746407, 0.7540134720837717852 ) ) ;
#16535 = DIRECTION ( 'NONE',  ( -2.412663730047099099E-15, 0.8967398287344627850, 0.4425581086832399147 ) ) ;
#16536 = CARTESIAN_POINT ( 'NONE',  ( 37.31647492878124694, -28.30384086642191477, 72.03616607671141026 ) ) ;
#16537 = CARTESIAN_POINT ( 'NONE',  ( 39.41296390513587511, -29.20384086642191335, 71.08074471024438878 ) ) ;
#16538 = EDGE_LOOP ( 'NONE', ( #12819, #9739, #913, #5594 ) ) ;
#16539 = PRODUCT_RELATED_PRODUCT_CATEGORY ( 'part', '', ( #11362 ) ) ;
#16540 = ORIENTED_EDGE ( 'NONE', *, *, #4207, .F. ) ;
#16541 = DIRECTION ( 'NONE',  ( -1.786044098272412642E-16, -0.4425581086832399702, 0.8967398287344628960 ) ) ;
#16542 = FACE_BOUND ( 'NONE', #18086, .T. ) ;
#16543 = DIRECTION ( 'NONE',  ( 1.000000000000000000, 0.000000000000000000, 0.000000000000000000 ) ) ;
#16544 = CARTESIAN_POINT ( 'NONE',  ( 36.49096545463212493, -8.103840866421908373, 71.32335560751963044 ) ) ;
#16545 = AXIS2_PLACEMENT_3D ( 'NONE', #4747, #614, #12368 ) ;
#16546 = APPLICATION_CONTEXT ( 'automotive_design' ) ;
#16547 = DIRECTION ( 'NONE',  ( -1.000000000000000000, 0.000000000000000000, 0.000000000000000000 ) ) ;
#16548 = AXIS2_PLACEMENT_3D ( 'NONE', #13863, #11947, #5751 ) ;
#16549 = CARTESIAN_POINT ( 'NONE',  ( 33.81606138205700063, 15.19123852234700323, 70.30501292736995822 ) ) ;
#16550 = ORIENTED_EDGE ( 'NONE', *, *, #4521, .T. ) ;
#16551 = ORIENTED_EDGE ( 'NONE', *, *, #19399, .F. ) ;
#16552 = ORIENTED_EDGE ( 'NONE', *, *, #25340, .F. ) ;
#16553 = DIRECTION ( 'NONE',  ( 1.836970198721029688E-16, 2.999999999999999839E-15, 1.000000000000000000 ) ) ;
#16554 = CARTESIAN_POINT ( 'NONE',  ( 38.82593461698262871, -8.913682088886101695, 69.62690120949091011 ) ) ;
#16555 = VECTOR ( 'NONE', #14164, 1000.000000000000227 ) ;
#16556 = VECTOR ( 'NONE', #8996, 1000.000000000000114 ) ;
#16557 = CARTESIAN_POINT ( 'NONE',  ( 36.31606138205700063, -16.77230293220685198, 77.52306850662458260 ) ) ;
#16558 = CARTESIAN_POINT ( 'NONE',  ( 40.81606138205700773, -24.05876147765400219, 74.30501292737008612 ) ) ;
#16559 = CARTESIAN_POINT ( 'NONE',  ( 43.81606138205700063, 44.92314894770294131, 80.37823623207322044 ) ) ;
#16560 = AXIS2_PLACEMENT_3D ( 'NONE', #8853, #22367, #4842 ) ;
#16561 = CARTESIAN_POINT ( 'NONE',  ( 36.31606138205702905, -21.82181003913287398, 31.95585308007613179 ) ) ;
#16562 = FACE_OUTER_BOUND ( 'NONE', #1489, .T. ) ;
#16563 = VECTOR ( 'NONE', #11400, 1000.000000000000000 ) ;
#16564 = DIRECTION ( 'NONE',  ( -2.048868001712896742E-15, 0.6595716529892345914, -0.7516416929448823669 ) ) ;
#16565 = EDGE_LOOP ( 'NONE', ( #16938, #8064, #15957, #10882 ) ) ;
#16566 = ORIENTED_EDGE ( 'NONE', *, *, #9727, .F. ) ;
#16568 = EDGE_CURVE ( 'NONE', #4444, #5522, #11728, .T. ) ;
#16567 = DIRECTION ( 'NONE',  ( -0.000000000000000000, -3.469446951953613400E-15, -1.000000000000000000 ) ) ;
#16569 = CARTESIAN_POINT ( 'NONE',  ( 37.50301148336529167, -27.11368208888610454, 69.06206559358663810 ) ) ;
#16570 = DIRECTION ( 'NONE',  ( 0.000000000000000000, 3.469446951953613400E-15, 1.000000000000000000 ) ) ;
#16571 = EDGE_CURVE ( 'NONE', #13311, #5909, #21498, .T. ) ;
#16572 = CARTESIAN_POINT ( 'NONE',  ( 38.37017380507020192, -16.01368208888609956, 72.51602215082118619 ) ) ;
#16573 = ORIENTED_EDGE ( 'NONE', *, *, #881, .F. ) ;
#16574 = AXIS2_PLACEMENT_3D ( 'NONE', #15424, #7579, #1621 ) ;
#16575 = ORIENTED_EDGE ( 'NONE', *, *, #17907, .F. ) ;
#16576 = DIRECTION ( 'NONE',  ( 2.312964634635742267E-15, -0.8967398287344627850, -0.4425581086832398592 ) ) ;
#16577 = CARTESIAN_POINT ( 'NONE',  ( 39.38009889167650357, -2.213682088886108179, 72.75271321436733274 ) ) ;
#16578 = CARTESIAN_POINT ( 'NONE',  ( 38.93987200065210175, -0.8038408664219099942, 72.33091598616827866 ) ) ;
#16579 = LINE ( 'NONE', #20454, #17810 ) ;
#16580 = VECTOR ( 'NONE', #5338, 1000.000000000000000 ) ;
#16581 = CARTESIAN_POINT ( 'NONE',  ( 37.61123632939165873, -9.913682088886107024, 73.73360434286902887 ) ) ;
#16582 = VECTOR ( 'NONE', #7130, 1000.000000000000000 ) ;
#16584 = ORIENTED_EDGE ( 'NONE', *, *, #16824, .T. ) ;
#16583 = CARTESIAN_POINT ( 'NONE',  ( 34.66606138205694521, 5.208890205473723611, 5.429380561359602453 ) ) ;
#16585 = CARTESIAN_POINT ( 'NONE',  ( 15.14989484155900001, 36.04731275961434989, 83.30501292736985874 ) ) ;
#16586 = EDGE_CURVE ( 'NONE', #14226, #17824, #17516, .T. ) ;
#16587 = AXIS2_PLACEMENT_3D ( 'NONE', #8259, #14431, #16100 ) ;
#16588 = LINE ( 'NONE', #22515, #11428 ) ;
#16589 = CYLINDRICAL_SURFACE ( 'NONE', #7919, 1.499999999999996669 ) ;
#16590 = LINE ( 'NONE', #9007, #366 ) ;
#16591 = AXIS2_PLACEMENT_3D ( 'NONE', #22578, #22328, #10871 ) ;
#16592 = CARTESIAN_POINT ( 'NONE',  ( 34.81606138205700773, -9.197413316359888569, 54.67416070422748220 ) ) ;
#16593 = PLANE ( 'NONE',  #2021 ) ;
#16594 = VERTEX_POINT ( 'NONE', #5785 ) ;
#16595 = DIRECTION ( 'NONE',  ( 0.000000000000000000, 0.5706330172266919076, -0.8212051873014208914 ) ) ;
#16596 = DIRECTION ( 'NONE',  ( 1.734723475976804876E-16, -1.163336342344335610E-15, 1.000000000000000000 ) ) ;
#16597 = ORIENTED_EDGE ( 'NONE', *, *, #22897, .T. ) ;
#16598 = ORIENTED_EDGE ( 'NONE', *, *, #21995, .T. ) ;
#16599 = VECTOR ( 'NONE', #8523, 1000.000000000000227 ) ;
#16600 = CARTESIAN_POINT ( 'NONE',  ( 40.26954217208372455, -16.90384086642191619, 72.86986841596734621 ) ) ;
#16601 = CIRCLE ( 'NONE', #5931, 1.000000000000000888 ) ;
#16602 = CARTESIAN_POINT ( 'NONE',  ( 39.82603832034400426, -22.31368208888610738, 72.40698646996133903 ) ) ;
#16603 = CARTESIAN_POINT ( 'NONE',  ( 31.91606138205697718, -5.022037326221728826, -5.474317061061731771 ) ) ;
#16604 = DIRECTION ( 'NONE',  ( -1.000000000000000000, 0.000000000000000000, 0.000000000000000000 ) ) ;
#16605 = SURFACE_STYLE_FILL_AREA ( #9024 ) ;
#16606 = VERTEX_POINT ( 'NONE', #5536 ) ;
#16607 = DIRECTION ( 'NONE',  ( 1.000000000000000000, 6.071532165918830747E-16, -1.734723475976829774E-16 ) ) ;
#16608 = CARTESIAN_POINT ( 'NONE',  ( 43.31606138205700063, -27.11289203277224402, 56.96090842897168471 ) ) ;
#16609 = CARTESIAN_POINT ( 'NONE',  ( 38.26194895904384197, 1.396159133578080080, 73.71602215082117482 ) ) ;
#16610 = VERTEX_POINT ( 'NONE', #13644 ) ;
#16611 = CARTESIAN_POINT ( 'NONE',  ( 34.81606138205700773, -14.36460986495925241, 36.24727600202827915 ) ) ;
#16612 = CARTESIAN_POINT ( 'NONE',  ( 41.31606138205687273, 43.19123852234595518, 61.30501292736988006 ) ) ;
#16613 =( GEOMETRIC_REPRESENTATION_CONTEXT ( 3 ) GLOBAL_UNCERTAINTY_ASSIGNED_CONTEXT ( ( #14664 ) ) GLOBAL_UNIT_ASSIGNED_CONTEXT ( ( #11413, #3537, #13351 ) ) REPRESENTATION_CONTEXT ( 'NONE', 'WORKASPACE' ) );
#16614 = CARTESIAN_POINT ( 'NONE',  ( 36.87297107704152666, -3.713682088886109511, 72.49904802271743165 ) ) ;
#16615 = CARTESIAN_POINT ( 'NONE',  ( 40.31606138205700063, 5.691238522346989903, 65.80501292736998664 ) ) ;
#16616 = EDGE_CURVE ( 'NONE', #19555, #18958, #7721, .T. ) ;
#16617 = CARTESIAN_POINT ( 'NONE',  ( 36.68196826583682935, -17.61368208888610454, 71.96809898377888715 ) ) ;
#16618 = AXIS2_PLACEMENT_3D ( 'NONE', #16679, #22602, #9345 ) ;
#16619 = AXIS2_PLACEMENT_3D ( 'NONE', #15907, #2371, #3003 ) ;
#16620 = DIRECTION ( 'NONE',  ( 0.000000000000000000, 0.8967398287344631180, 0.4425581086832395261 ) ) ;
#16621 = VECTOR ( 'NONE', #24773, 1000.000000000000000 ) ;
#16622 = CARTESIAN_POINT ( 'NONE',  ( 46.91606138205695231, 1.152853241805996021, -2.169147274601560760 ) ) ;
#16623 = CARTESIAN_POINT ( 'NONE',  ( 38.37017380507018771, -19.60384086642191193, 70.24448340153875847 ) ) ;
#16624 = CARTESIAN_POINT ( 'NONE',  ( 40.14115730948191185, -4.513682088886103116, 71.32335560751961623 ) ) ;
#16625 = ORIENTED_EDGE ( 'NONE', *, *, #18303, .T. ) ;
#16626 = CARTESIAN_POINT ( 'NONE',  ( 33.72038411900453525, 3.276404855341403355, 6.354292672466786307 ) ) ;
#16627 = ORIENTED_EDGE ( 'NONE', *, *, #25130, .F. ) ;
#16628 = CARTESIAN_POINT ( 'NONE',  ( 36.68196826583682935, -6.003840866421913169, 70.79240656858108593 ) ) ;
#16629 = EDGE_CURVE ( 'NONE', #17824, #4719, #14564, .T. ) ;
#16630 = DIRECTION ( 'NONE',  ( 0.000000000000000000, 0.8212051873014208914, 0.5706330172266919076 ) ) ;
#16631 = PRODUCT_DEFINITION_FORMATION_WITH_SPECIFIED_SOURCE ( 'ANY', '', #1662, .NOT_KNOWN. ) ;
#16632 = EDGE_CURVE ( 'NONE', #18444, #10990, #19185, .T. ) ;
#16633 = CARTESIAN_POINT ( 'NONE',  ( 39.98359781491296161, -2.413682088886103472, 71.86517103874048473 ) ) ;
#16634 = ORIENTED_EDGE ( 'NONE', *, *, #15292, .F. ) ;
#16635 = CARTESIAN_POINT ( 'NONE',  ( 36.36258059203031934, -7.713682088886110400, 72.86986841596736042 ) ) ;
#16636 = EDGE_LOOP ( 'NONE', ( #2662, #1907, #23390, #4102, #4815, #1129, #23224, #745, #10671, #1473, #5630, #5752 ) ) ;
#16637 = DIRECTION ( 'NONE',  ( -2.574571254471601357E-15, 0.8967398287344627850, 0.4425581086832399147 ) ) ;
#16638 = EDGE_CURVE ( 'NONE', #12758, #21730, #17254, .T. ) ;
#16639 = AXIS2_PLACEMENT_3D ( 'NONE', #18088, #14461, #16131 ) ;
#16640 = CARTESIAN_POINT ( 'NONE',  ( 39.24876120206129571, -14.90384086642191264, 72.12822762946747446 ) ) ;
#16641 = EDGE_CURVE ( 'NONE', #1701, #9149, #20997, .T. ) ;
#16642 = EDGE_CURVE ( 'NONE', #6874, #22610, #10040, .T. ) ;
#16643 = ORIENTED_EDGE ( 'NONE', *, *, #21723, .T. ) ;
#16644 = EDGE_LOOP ( 'NONE', ( #23343, #21931, #17246, #23755 ) ) ;
#16645 = FACE_BOUND ( 'NONE', #9427, .T. ) ;
#16646 = CARTESIAN_POINT ( 'NONE',  ( 36.31606138205700063, 43.19123852234596939, 65.30501292736988717 ) ) ;
#16647 = CARTESIAN_POINT ( 'NONE',  ( 36.29569395875881099, -16.30384086642192187, 72.77780686321128201 ) ) ;
#16648 = AXIS2_PLACEMENT_3D ( 'NONE', #21034, #21160, #18584 ) ;
#16649 = CARTESIAN_POINT ( 'NONE',  ( 36.51558096900348005, -21.15836054580815784, 75.86898487248532774 ) ) ;
#16650 = SURFACE_STYLE_USAGE ( .BOTH. , #22952 ) ;
#16651 = CARTESIAN_POINT ( 'NONE',  ( 38.82593461698262871, -18.91368208888609459, 69.62690120949091011 ) ) ;
#16652 = LINE ( 'NONE', #11118, #10905 ) ;
#16653 = EDGE_CURVE ( 'NONE', #7328, #2134, #967, .T. ) ;
#16654 = CARTESIAN_POINT ( 'NONE',  ( 30.81606138205698642, -6.382952266546177533, -7.235923851661291373 ) ) ;
#16655 = EDGE_CURVE ( 'NONE', #17608, #5806, #10868, .T. ) ;
#16656 = ORIENTED_EDGE ( 'NONE', *, *, #109, .F. ) ;
#16657 = DIRECTION ( 'NONE',  ( -1.000000000000000000, -1.734723475976804876E-16, 1.734723475976814737E-16 ) ) ;
#16658 = DIRECTION ( 'NONE',  ( 0.000000000000000000, 1.000000000000000000, -3.469446951953613794E-15 ) ) ;
#16659 = CARTESIAN_POINT ( 'NONE',  ( 39.38009889167648936, -15.40384086642190908, 70.00779233799262613 ) ) ;
#16660 = VECTOR ( 'NONE', #875, 1000.000000000000000 ) ;
#16661 = CARTESIAN_POINT ( 'NONE',  ( 0.000000000000000000, 0.000000000000000000, 0.000000000000000000 ) ) ;
#16662 = CARTESIAN_POINT ( 'NONE',  ( 31.81606138205700418, -21.15876147765410309, 66.30501292737000085 ) ) ;
#16663 = CARTESIAN_POINT ( 'NONE',  ( 36.49096545463212493, -27.51368208888610312, 71.43714994484030001 ) ) ;
#16664 = LINE ( 'NONE', #20660, #10656 ) ;
#16665 = CARTESIAN_POINT ( 'NONE',  ( 33.31606138205700773, -19.47805968271055477, 24.94720442500192448 ) ) ;
#16666 = CARTESIAN_POINT ( 'NONE',  ( 39.82603832034400426, -23.30384086642190766, 70.35351908239857721 ) ) ;
#16667 = DIRECTION ( 'NONE',  ( -1.000000000000000000, -1.187136597504755470E-16, -8.249087426255173666E-17 ) ) ;
#16668 = ORIENTED_EDGE ( 'NONE', *, *, #11729, .T. ) ;
#16669 = CARTESIAN_POINT ( 'NONE',  ( 39.98359781491296161, -22.41368208888610525, 71.86517103874047052 ) ) ;
#16670 = ORIENTED_EDGE ( 'NONE', *, *, #25440, .T. ) ;
#16671 = ORIENTED_EDGE ( 'NONE', *, *, #7512, .F. ) ;
#16672 = PLANE ( 'NONE',  #10289 ) ;
#16673 = DIRECTION ( 'NONE',  ( -0.000000000000000000, -0.7540134720837717852, -0.6568589528324747517 ) ) ;
#16674 = CARTESIAN_POINT ( 'NONE',  ( 38.73920764526925353, -0.1136820888861002354, 72.49843995877331793 ) ) ;
#16675 = ADVANCED_FACE ( 'NONE', ( #22479 ), #15697, .T. ) ;
#16676 = CARTESIAN_POINT ( 'NONE',  ( 39.24876120206128860, -0.7136820888861000745, 70.63227792289247020 ) ) ;
#16677 = ORIENTED_EDGE ( 'NONE', *, *, #10274, .F. ) ;
#16678 = ORIENTED_EDGE ( 'NONE', *, *, #7053, .T. ) ;
#16679 = CARTESIAN_POINT ( 'NONE',  ( 38.31606138205700063, 38.19123852234599781, 71.30501292737001506 ) ) ;
#16680 = DIRECTION ( 'NONE',  ( -1.000000000000000000, 1.508529456107831862E-16, 1.048235847051697233E-16 ) ) ;
#16681 = ORIENTED_EDGE ( 'NONE', *, *, #24048, .T. ) ;
#16682 = DIRECTION ( 'NONE',  ( -2.168404344971010101E-16, 0.8212051873014210024, 0.5706330172266920187 ) ) ;
#16683 = CARTESIAN_POINT ( 'NONE',  ( 38.93415946300896024, -1.503840866421908729, 69.66206559358663242 ) ) ;
#16684 = AXIS2_PLACEMENT_3D ( 'NONE', #16348, #18308, #16099 ) ;
#16685 = CARTESIAN_POINT ( 'NONE',  ( 40.31606138205700773, 43.19123852234596939, 66.30501292736988717 ) ) ;
#16686 = PLANE ( 'NONE',  #22098 ) ;
#16687 = ORIENTED_EDGE ( 'NONE', *, *, #10244, .T. ) ;
#16688 = EDGE_LOOP ( 'NONE', ( #17384, #1867, #18481, #24800 ) ) ;
#16689 = DIRECTION ( 'NONE',  ( -1.327674326049719602E-15, 0.4425581086832399147, -0.8967398287344627850 ) ) ;
#16690 = CARTESIAN_POINT ( 'NONE',  ( 37.69796330110504101, -3.113682088886099208, 69.66206559358664663 ) ) ;
#16691 = EDGE_LOOP ( 'NONE', ( #18994, #24472, #14557, #20479 ) ) ;
#16692 = DIRECTION ( 'NONE',  ( -3.491481338843135327E-15, -1.000000000000000000, 3.000000000000000628E-15 ) ) ;
#16693 = SURFACE_SIDE_STYLE ('',( #14167 ) ) ;
#16694 = DIRECTION ( 'NONE',  ( -1.000000000000000000, -2.452751524064188892E-15, -1.339444584486322859E-15 ) ) ;
#16695 = DIRECTION ( 'NONE',  ( 0.000000000000000000, -2.999999999999999839E-15, -1.000000000000000000 ) ) ;
#16696 = ADVANCED_FACE ( 'NONE', ( #8585 ), #21628, .T. ) ;
#16697 = DIRECTION ( 'NONE',  ( 0.000000000000000000, 0.000000000000000000, -1.000000000000000000 ) ) ;
#16698 = LINE ( 'NONE', #20437, #12345 ) ;
#16699 = CARTESIAN_POINT ( 'NONE',  ( 40.31606138205700773, 37.44123852234599781, 75.30501292736990138 ) ) ;
#16700 = CYLINDRICAL_SURFACE ( 'NONE', #6224, 0.7500000000000006661 ) ;
#16701 = ORIENTED_EDGE ( 'NONE', *, *, #1667, .T. ) ;
#16702 = VERTEX_POINT ( 'NONE', #449 ) ;
#16703 = CARTESIAN_POINT ( 'NONE',  ( 43.31606138205700063, -12.76023008545320181, 21.53290024082827969 ) ) ;
#16704 = DIRECTION ( 'NONE',  ( -1.000000000000000000, -3.091505625455829092E-15, -4.515976121274730398E-17 ) ) ;
#16705 = APPLICATION_CONTEXT ( 'automotive_design' ) ;
#16706 = CARTESIAN_POINT ( 'NONE',  ( 38.93987200065208754, -14.81368208888610205, 70.42958956619168021 ) ) ;
#16707 = VERTEX_POINT ( 'NONE', #16421 ) ;
#16708 = ORIENTED_EDGE ( 'NONE', *, *, #11171, .F. ) ;
#16709 = CARTESIAN_POINT ( 'NONE',  ( 33.31606138205700773, 3.392460599465057403, 64.84545171350526971 ) ) ;
#16710 = CARTESIAN_POINT ( 'NONE',  ( 36.87297107704152666, 0.2863179111138939303, 72.49904802271743165 ) ) ;
#16711 = CARTESIAN_POINT ( 'NONE',  ( 37.80618814713138676, -21.70384086642190979, 69.62690120949091011 ) ) ;
#16712 = CARTESIAN_POINT ( 'NONE',  ( 33.56606138205700773, 43.19123852234599781, 74.30501292736987295 ) ) ;
#16713 = CARTESIAN_POINT ( 'NONE',  ( 35.86008812008917346, -9.513682088886103116, 71.43714994484035685 ) ) ;
#16714 = DIRECTION ( 'NONE',  ( 1.000000000000000000, 2.999999999999999839E-15, 0.000000000000000000 ) ) ;
#16715 = LINE ( 'NONE', #18911, #5453 ) ;
#16716 = DIRECTION ( 'NONE',  ( 0.000000000000000000, 3.469446951953613400E-15, 1.000000000000000000 ) ) ;
#16717 = EDGE_CURVE ( 'NONE', #24103, #15157, #3865, .T. ) ;
#16718 = CARTESIAN_POINT ( 'NONE',  ( 36.31606138205700063, -30.30876147765400574, 73.55501292737010033 ) ) ;
#16719 = EDGE_CURVE ( 'NONE', #17700, #7542, #164, .T. ) ;
#16720 = CARTESIAN_POINT ( 'NONE',  ( 38.83610899671118943, -5.265395967213828854, 82.79985564382789676 ) ) ;
#16721 = CARTESIAN_POINT ( 'NONE',  ( 39.66066260159759338, -29.10876147765399224, 69.64448340153876416 ) ) ;
#16722 = ADVANCED_FACE ( 'NONE', ( #23545 ), #22356, .F. ) ;
#16723 = DIRECTION ( 'NONE',  ( 0.000000000000000000, 0.6568589528324746407, -0.7540134720837716742 ) ) ;
#16724 = ORIENTED_EDGE ( 'NONE', *, *, #19451, .T. ) ;
#16725 = DIRECTION ( 'NONE',  ( 0.000000000000000000, 0.6568589528324746407, -0.7540134720837717852 ) ) ;
#16726 = MANIFOLD_SOLID_BREP ( 'NONE', #14693 ) ;
#16727 = CARTESIAN_POINT ( 'NONE',  ( 39.81606138205700063, -4.070846987468769385, 59.14016975459033887 ) ) ;
#16728 = ORIENTED_EDGE ( 'NONE', *, *, #19356, .F. ) ;
#16729 = ORIENTED_EDGE ( 'NONE', *, *, #2858, .F. ) ;
#16730 = UNCERTAINTY_MEASURE_WITH_UNIT (LENGTH_MEASURE( 1.000000000000000082E-05 ), #11026, 'distance_accuracy_value', 'NONE');
#16731 = CARTESIAN_POINT ( 'NONE',  ( 39.02088643472237806, -18.70384086642192045, 73.73360434286898624 ) ) ;
#16732 = EDGE_CURVE ( 'NONE', #13486, #23038, #17771, .T. ) ;
#16733 = CARTESIAN_POINT ( 'NONE',  ( 39.38009889167650357, -20.21368208888610951, 72.75271321436731853 ) ) ;
#16734 = DIRECTION ( 'NONE',  ( 1.000000000000000000, 8.911169920151748851E-16, 3.114923731923493702E-16 ) ) ;
#16735 = DIRECTION ( 'NONE',  ( 2.690219486203388234E-15, -0.8967398287344627850, -0.4425581086832399147 ) ) ;
#16736 = FILL_AREA_STYLE ('',( #17001 ) ) ;
#16737 = ORIENTED_EDGE ( 'NONE', *, *, #13974, .F. ) ;
#16738 = DIRECTION ( 'NONE',  ( 0.000000000000000000, -1.000000000000000000, 3.115648231731786715E-15 ) ) ;
#16739 = CARTESIAN_POINT ( 'NONE',  ( 38.48938833801555148, 38.69123852234600491, 72.28987726642293410 ) ) ;
#16740 = CARTESIAN_POINT ( 'NONE',  ( 36.29569395875879678, -25.31368208888610027, 69.98269868914866265 ) ) ;
#16741 = AXIS2_PLACEMENT_3D ( 'NONE', #4718, #17876, #10261 ) ;
#16742 = VERTEX_POINT ( 'NONE', #14253 ) ;
#16743 = CARTESIAN_POINT ( 'NONE',  ( 43.81606138205700063, -39.23120981750657421, 69.49370132789680099 ) ) ;
#16744 = AXIS2_PLACEMENT_3D ( 'NONE', #8931, #18462, #16775 ) ;
#16745 = CARTESIAN_POINT ( 'NONE',  ( 39.29254315202756231, -0.8136820888860994971, 69.94417936956673998 ) ) ;
#16746 = DIRECTION ( 'NONE',  ( 0.000000000000000000, 0.000000000000000000, 1.000000000000000000 ) ) ;
#16747 = CARTESIAN_POINT ( 'NONE',  ( 36.64852494920107517, -23.41368208888610525, 70.89533451361945993 ) ) ;
#16748 = CARTESIAN_POINT ( 'NONE',  ( 40.11656585159207822, -21.15771639874553500, 75.86402839307550039 ) ) ;
#16749 = CARTESIAN_POINT ( 'NONE',  ( 44.81606138205700063, -38.55876147765400930, 73.30501292737012875 ) ) ;
#16750 = CARTESIAN_POINT ( 'NONE',  ( 38.26194895904384197, -18.60384086642190837, 72.51602215082118619 ) ) ;
#16751 = CARTESIAN_POINT ( 'NONE',  ( 36.68196826583682935, -3.613682088886103205, 71.96809898377890136 ) ) ;
#16752 = LINE ( 'NONE', #22556, #23812 ) ;
#16753 = EDGE_LOOP ( 'NONE', ( #21607, #7975, #20834, #3218, #4776, #3143, #17563, #7666, #15197, #10530 ) ) ;
#16754 = CLOSED_SHELL ( 'NONE', ( #3807, #21469, #16338, #24873, #9597 ) ) ;
#16755 = CARTESIAN_POINT ( 'NONE',  ( 37.69796330110505522, -2.503840866421913613, 73.09843995877331224 ) ) ;
#16756 = DIRECTION ( 'NONE',  ( 0.000000000000000000, -1.000000000000000000, 3.469446951953613794E-15 ) ) ;
#16757 = AXIS2_PLACEMENT_3D ( 'NONE', #22960, #20911, #20523 ) ;
#16758 = VECTOR ( 'NONE', #17883, 1000.000000000000000 ) ;
#16759 = EDGE_CURVE ( 'NONE', #22610, #1644, #16202, .T. ) ;
#16760 = CARTESIAN_POINT ( 'NONE',  ( 37.80618814713140097, -5.913682088886107024, 73.13360434286904876 ) ) ;
#16761 = VERTEX_POINT ( 'NONE', #6772 ) ;
#16762 = CARTESIAN_POINT ( 'NONE',  ( 36.29569395875879678, -11.31368208888609850, 69.98269868914867686 ) ) ;
#16763 = ORIENTED_EDGE ( 'NONE', *, *, #13490, .F. ) ;
#16764 = PLANE ( 'NONE',  #9907 ) ;
#16765 = CARTESIAN_POINT ( 'NONE',  ( 37.69225076346193504, -9.803840866421911215, 70.42958956619168021 ) ) ;
#16766 = LINE ( 'NONE', #1168, #13476 ) ;
#16767 = ORIENTED_EDGE ( 'NONE', *, *, #18309, .T. ) ;
#16768 = DIRECTION ( 'NONE',  ( 0.000000000000000000, 6.938893903907222067E-15, -1.000000000000000000 ) ) ;
#16769 = DIRECTION ( 'NONE',  ( -1.445602896647339903E-16, 1.000000000000000000, -2.999999999999999839E-15 ) ) ;
#16770 = CARTESIAN_POINT ( 'NONE',  ( 39.12911128074872380, -19.50384086642191406, 69.06206559358665231 ) ) ;
#16771 = DIRECTION ( 'NONE',  ( -0.000000000000000000, 0.5735764363510447161, -0.8191520442889929088 ) ) ;
#16772 = PLANE ( 'NONE',  #15706 ) ;
#16773 = CARTESIAN_POINT ( 'NONE',  ( 36.68196826583682935, -17.61368208888610454, 71.96809898377888715 ) ) ;
#16774 = CARTESIAN_POINT ( 'NONE',  ( 46.81606138205707168, -35.90387122078352178, 69.64117576433150703 ) ) ;
#16775 = DIRECTION ( 'NONE',  ( 0.000000000000000000, -0.3299742535180970049, 0.9439899321577400748 ) ) ;
#16776 = VECTOR ( 'NONE', #6446, 1000.000000000000000 ) ;
#16777 = EDGE_CURVE ( 'NONE', #1954, #12862, #6516, .T. ) ;
#16778 = EDGE_LOOP ( 'NONE', ( #528, #10785, #24289, #17148 ) ) ;
#16779 = AXIS2_PLACEMENT_3D ( 'NONE', #24611, #2984, #923 ) ;
#16780 = VECTOR ( 'NONE', #23782, 1000.000000000000000 ) ;
#16781 = LINE ( 'NONE', #12432, #12503 ) ;
#16782 = EDGE_CURVE ( 'NONE', #21068, #12825, #4830, .T. ) ;
#16783 = DIRECTION ( 'NONE',  ( 0.000000000000000000, -0.4425581086832348077, 0.8967398287344653385 ) ) ;
#16784 = CARTESIAN_POINT ( 'NONE',  ( 39.75915168707251723, -14.90384086642191264, 72.49904802271738902 ) ) ;
#16785 = CARTESIAN_POINT ( 'NONE',  ( 0.000000000000000000, 0.000000000000000000, 0.000000000000000000 ) ) ;
#16786 = CARTESIAN_POINT ( 'NONE',  ( 33.56606138205700773, 43.19123852234599781, 75.30501292736987295 ) ) ;
#16787 = ADVANCED_FACE ( 'NONE', ( #955 ), #18615, .F. ) ;
#16788 = CARTESIAN_POINT ( 'NONE',  ( 36.68196826583682935, -23.61368208888610454, 71.96809898377887293 ) ) ;
#16789 = DIRECTION ( 'NONE',  ( -1.000000000000000000, 0.000000000000000000, 0.000000000000000000 ) ) ;
#16790 = CARTESIAN_POINT ( 'NONE',  ( 39.82603832034400426, -27.30384086642191122, 70.35351908239857721 ) ) ;
#16791 = CARTESIAN_POINT ( 'NONE',  ( 38.18531088334250967, -5.204193249396280585, 82.80501292736992980 ) ) ;
#16792 = EDGE_CURVE ( 'NONE', #10061, #8601, #14869, .T. ) ;
#16793 = CARTESIAN_POINT ( 'NONE',  ( 39.29254315202756231, -24.81368208888610383, 69.94417936956671156 ) ) ;
#16794 = VERTEX_POINT ( 'NONE', #22731 ) ;
#16795 = ORIENTED_EDGE ( 'NONE', *, *, #8581, .F. ) ;
#16796 = CYLINDRICAL_SURFACE ( 'NONE', #8228, 1.099999999999999867 ) ;
#16797 = CARTESIAN_POINT ( 'NONE',  ( 40.31606138205700773, 37.94123852234599070, 73.55501292736988717 ) ) ;
#16798 = CARTESIAN_POINT ( 'NONE',  ( 37.21915885897815457, -1.413682088886099253, 71.08074471024443142 ) ) ;
#16799 = AXIS2_PLACEMENT_3D ( 'NONE', #20693, #3029, #24786 ) ;
#16800 = CARTESIAN_POINT ( 'NONE',  ( 38.63098279924288647, 1.086317911113899415, 70.22690120949094705 ) ) ;
#16801 = ORIENTED_EDGE ( 'NONE', *, *, #15855, .T. ) ;
#16802 = VERTEX_POINT ( 'NONE', #16809 ) ;
#16803 = LINE ( 'NONE', #24636, #12120 ) ;
#16804 = DIRECTION ( 'NONE',  ( 2.690219486203388234E-15, -0.8967398287344627850, -0.4425581086832399147 ) ) ;
#16805 = ORIENTED_EDGE ( 'NONE', *, *, #5485, .T. ) ;
#16806 = CARTESIAN_POINT ( 'NONE',  ( 44.06606138205700063, 47.04446929126260102, 81.37823623207319201 ) ) ;
#16807 = CARTESIAN_POINT ( 'NONE',  ( 36.80608444377001831, -2.303840866421914768, 72.40698646996136745 ) ) ;
#16808 = CIRCLE ( 'NONE', #16387, 1.100000000000000089 ) ;
#16809 = CARTESIAN_POINT ( 'NONE',  ( 42.68042513965293949, 2.191238522347003226, 70.30501292737000085 ) ) ;
#16810 = DIRECTION ( 'NONE',  ( 0.000000000000000000, -0.5706330172266915746, 0.8212051873014213355 ) ) ;
#16811 = ORIENTED_EDGE ( 'NONE', *, *, #21588, .F. ) ;
#16812 = VERTEX_POINT ( 'NONE', #3408 ) ;
#16813 = VECTOR ( 'NONE', #13708, 1000.000000000000000 ) ;
#16814 = EDGE_CURVE ( 'NONE', #4130, #9093, #22388, .T. ) ;
#16815 = ORIENTED_EDGE ( 'NONE', *, *, #1903, .T. ) ;
#16816 = CARTESIAN_POINT ( 'NONE',  ( 43.81606138205700063, 35.44123852234597649, 68.30501292736990138 ) ) ;
#16817 = ADVANCED_FACE ( 'NONE', ( #20935 ), #12832, .T. ) ;
#16818 = CARTESIAN_POINT ( 'NONE',  ( 39.29254315202756231, -2.813682088886101162, 69.94417936956673998 ) ) ;
#16819 = ORIENTED_EDGE ( 'NONE', *, *, #11618, .T. ) ;
#16820 = DIRECTION ( 'NONE',  ( 1.000000000000000000, 2.168404344971010101E-16, -1.734723475976814737E-16 ) ) ;
#16821 = ADVANCED_FACE ( 'NONE', ( #18748 ), #5470, .F. ) ;
#16822 = DIRECTION ( 'NONE',  ( -2.122643018205887308E-17, 1.000000000000000000, -3.120611096041553009E-15 ) ) ;
#16823 = ADVANCED_FACE ( 'NONE', ( #1471 ), #7277, .T. ) ;
#16824 = EDGE_CURVE ( 'NONE', #1986, #562, #17334, .T. ) ;
#16825 = AXIS2_PLACEMENT_3D ( 'NONE', #22842, #5203, #10999 ) ;
#16826 = CARTESIAN_POINT ( 'NONE',  ( 33.31606138205700773, -5.204193249396356968, 72.80501292736992980 ) ) ;
#16827 = DIRECTION ( 'NONE',  ( 1.000000000000000000, 1.734723475976799945E-16, -1.734723475976814737E-16 ) ) ;
#16828 = DIRECTION ( 'NONE',  ( 1.000000000000000000, 0.000000000000000000, 0.000000000000000000 ) ) ;
#16829 = CARTESIAN_POINT ( 'NONE',  ( 33.40064408022072939, 41.43850569188389699, 79.87823623207322044 ) ) ;
#16830 = PRESENTATION_STYLE_ASSIGNMENT (( #14885 ) ) ;
#16831 = EDGE_CURVE ( 'NONE', #1002, #22555, #1080, .T. ) ;
#16832 = CYLINDRICAL_SURFACE ( 'NONE', #13227, 0.5000000000000004441 ) ;
#16833 = ORIENTED_EDGE ( 'NONE', *, *, #13505, .T. ) ;
#16834 = ORIENTED_EDGE ( 'NONE', *, *, #18912, .F. ) ;
#16835 = DIRECTION ( 'NONE',  ( 0.000000000000000000, 0.9992330079037401447, -0.03915859951075795903 ) ) ;
#16836 = AXIS2_PLACEMENT_3D ( 'NONE', #17026, #22932, #13163 ) ;
#16837 = LINE ( 'NONE', #16963, #15604 ) ;
#16838 = CARTESIAN_POINT ( 'NONE',  ( 38.93987200065208754, -18.81368208888610027, 70.42958956619168021 ) ) ;
#16839 = ORIENTED_EDGE ( 'NONE', *, *, #6086, .T. ) ;
#16840 = VERTEX_POINT ( 'NONE', #17200 ) ;
#16841 = CARTESIAN_POINT ( 'NONE',  ( 38.31606138205700063, -5.204193249396280585, 82.80501292736992980 ) ) ;
#16842 = CARTESIAN_POINT ( 'NONE',  ( 39.82603832034400426, -0.3136820888861094336, 72.40698646996135324 ) ) ;
#16843 = CARTESIAN_POINT ( 'NONE',  ( 37.25202387243754032, -26.40384086642191619, 72.75271321436730432 ) ) ;
#16844 = AXIS2_PLACEMENT_3D ( 'NONE', #12025, #3760, #17558 ) ;
#16845 = CARTESIAN_POINT ( 'NONE',  ( 45.81606138205700063, 34.92314894770294131, 81.17823623207323180 ) ) ;
#16846 = EDGE_CURVE ( 'NONE', #18113, #21608, #17470, .T. ) ;
#16847 = CARTESIAN_POINT ( 'NONE',  ( 40.55423172469004811, -10.41368208888610347, 72.05058123536544201 ) ) ;
#16848 = VECTOR ( 'NONE', #7605, 1000.000000000000227 ) ;
#16849 = CARTESIAN_POINT ( 'NONE',  ( 34.06606138205700773, -37.81581049437287589, 70.47722359350073873 ) ) ;
#16850 = VERTEX_POINT ( 'NONE', #17078 ) ;
#16851 = CARTESIAN_POINT ( 'NONE',  ( 33.31606138205700773, 6.294683054830111146, 7.131205101789720224 ) ) ;
#16852 = LINE ( 'NONE', #20459, #22934 ) ;
#16853 = DIRECTION ( 'NONE',  ( 1.000000000000000000, -3.299634970502069713E-17, 4.748546390019022251E-17 ) ) ;
#16854 = VECTOR ( 'NONE', #20320, 1000.000000000000000 ) ;
#16855 = CIRCLE ( 'NONE', #23426, 0.5000000000000004441 ) ;
#16856 = DIRECTION ( 'NONE',  ( -1.734723475976814737E-16, 1.000000000000000000, -3.491481338843135327E-15 ) ) ;
#16857 = CARTESIAN_POINT ( 'NONE',  ( 33.40064408022072939, 41.67000142393845152, 79.52109337493035923 ) ) ;
#16858 = PLANE ( 'NONE',  #12727 ) ;
#16859 = AXIS2_PLACEMENT_3D ( 'NONE', #16462, #10691, #19050 ) ;
#16860 = ORIENTED_EDGE ( 'NONE', *, *, #19884, .T. ) ;
#16861 = DIRECTION ( 'NONE',  ( -1.000000000000000000, -2.452751524064188892E-15, -1.339444584486322859E-15 ) ) ;
#16862 = CARTESIAN_POINT ( 'NONE',  ( 40.31606138205700773, -30.30876147765399864, 75.30501292736995822 ) ) ;
#16863 = ORIENTED_EDGE ( 'NONE', *, *, #8448, .T. ) ;
#16864 = ORIENTED_EDGE ( 'NONE', *, *, #13806, .T. ) ;
#16865 = CARTESIAN_POINT ( 'NONE',  ( 36.29569395875881099, -16.30384086642192187, 72.77780686321128201 ) ) ;
#16866 = VECTOR ( 'NONE', #22344, 1000.000000000000000 ) ;
#16867 = CARTESIAN_POINT ( 'NONE',  ( 36.64852494920107517, -21.41368208888610525, 70.89533451361947414 ) ) ;
#16868 = CARTESIAN_POINT ( 'NONE',  ( 34.81606138205700773, -20.93319939328399926, 43.78741072286599945 ) ) ;
#16869 = EDGE_CURVE ( 'NONE', #14544, #13705, #13215, .T. ) ;
#16870 = AXIS2_PLACEMENT_3D ( 'NONE', #12058, #14234, #2490 ) ;
#16871 = EDGE_CURVE ( 'NONE', #5334, #20374, #19130, .T. ) ;
#16872 = CARTESIAN_POINT ( 'NONE',  ( 41.06606138205702194, -20.30191568716147898, 23.22716926412510219 ) ) ;
#16873 = SURFACE_STYLE_USAGE ( .BOTH. , #11209 ) ;
#16874 = VERTEX_POINT ( 'NONE', #24896 ) ;
#16875 = CARTESIAN_POINT ( 'NONE',  ( 32.81606138205700773, -38.55876147765401640, 71.30501292737012875 ) ) ;
#16876 = DIRECTION ( 'NONE',  ( 5.047295537021760406E-31, -1.000000000000000000, 3.491481338843135327E-15 ) ) ;
#16877 = CARTESIAN_POINT ( 'NONE',  ( 40.52078840805428683, -26.61368208888610809, 70.60699637195608602 ) ) ;
#16878 = VERTEX_POINT ( 'NONE', #21190 ) ;
#16879 = DIRECTION ( 'NONE',  ( 0.000000000000000000, 2.999999999999999839E-15, 1.000000000000000000 ) ) ;
#16880 = CARTESIAN_POINT ( 'NONE',  ( 36.64852494920107517, 0.5863179111138955291, 70.89533451361948835 ) ) ;
#16881 = PLANE ( 'NONE',  #3816 ) ;
#16882 = CARTESIAN_POINT ( 'NONE',  ( 39.82603832034401847, -20.31368208888610738, 72.40698646996131060 ) ) ;
#16883 = VECTOR ( 'NONE', #24598, 1000.000000000000114 ) ;
#16884 = DIRECTION ( 'NONE',  ( -2.011972697750612571E-15, 0.6595716529892353686, -0.7516416929448815898 ) ) ;
#16885 = EDGE_CURVE ( 'NONE', #19940, #2302, #1212, .T. ) ;
#16886 = CARTESIAN_POINT ( 'NONE',  ( 38.31606138205700063, -5.204193249396277032, 83.30501292736992980 ) ) ;
#16887 = AXIS2_PLACEMENT_3D ( 'NONE', #10811, #2931, #7205 ) ;
#16888 = CARTESIAN_POINT ( 'NONE',  ( 39.41296390513587511, -19.20384086642191335, 71.08074471024441721 ) ) ;
#16889 = CARTESIAN_POINT ( 'NONE',  ( 40.14115730948191185, -8.513682088886104893, 71.32335560751961623 ) ) ;
#16890 = ORIENTED_EDGE ( 'NONE', *, *, #7183, .F. ) ;
#16891 = CARTESIAN_POINT ( 'NONE',  ( 34.56606138205700773, 42.19123852234599781, 74.30501292736987295 ) ) ;
#16892 = ORIENTED_EDGE ( 'NONE', *, *, #10224, .T. ) ;
#16893 = CARTESIAN_POINT ( 'NONE',  ( 36.80608444377001831, -6.303840866421912104, 72.40698646996136745 ) ) ;
#16894 = CARTESIAN_POINT ( 'NONE',  ( 43.81606138205700063, 28.69846577177642288, 66.12638289304319983 ) ) ;
#16895 = CARTESIAN_POINT ( 'NONE',  ( 36.80608444377001121, -5.313682088886100274, 70.35351908239860563 ) ) ;
#16896 = ORIENTED_EDGE ( 'NONE', *, *, #19347, .T. ) ;
#16897 = CARTESIAN_POINT ( 'NONE',  ( 39.64521430340304420, -6.813682088886101162, 69.45876917294177133 ) ) ;
#16898 = ORIENTED_EDGE ( 'NONE', *, *, #1627, .T. ) ;
#16899 = LINE ( 'NONE', #7108, #24278 ) ;
#16900 = ADVANCED_FACE ( 'NONE', ( #24643 ), #7021, .T. ) ;
#16901 = CARTESIAN_POINT ( 'NONE',  ( 38.00113996487112189, -9.703840866421911571, 70.22690120949091863 ) ) ;
#16902 = ADVANCED_FACE ( 'NONE', ( #22860 ), #1343, .F. ) ;
#16903 = DIRECTION ( 'NONE',  ( 9.999999999999998805E-16, -0.9439899321577399638, -0.3299742535180969494 ) ) ;
#16904 = CIRCLE ( 'NONE', #23066, 4.000000000000000000 ) ;
#16905 = ORIENTED_EDGE ( 'NONE', *, *, #18849, .F. ) ;
#16906 = CARTESIAN_POINT ( 'NONE',  ( 33.81606138205700063, 2.191238522347003226, 70.30501292737000085 ) ) ;
#16907 = MANIFOLD_SOLID_BREP ( 'NONE', #11017 ) ;
#16908 = CARTESIAN_POINT ( 'NONE',  ( 45.81606138205707168, -37.70325315460877391, 65.37863370302704880 ) ) ;
#16909 = CARTESIAN_POINT ( 'NONE',  ( 40.26954217208372455, -16.90384086642191619, 72.86986841596734621 ) ) ;
#16910 = AXIS2_PLACEMENT_3D ( 'NONE', #1483, #17596, #5368 ) ;
#16911 = CARTESIAN_POINT ( 'NONE',  ( 36.57656417722905928, -21.21640831487187739, 75.34994987701170999 ) ) ;
#16912 = DIRECTION ( 'NONE',  ( 1.169972191870009723E-15, -0.4425581086832399147, 0.8967398287344627850 ) ) ;
#16913 = CARTESIAN_POINT ( 'NONE',  ( 37.33957961208646736, -17.81368208888611093, 72.81632618279321889 ) ) ;
#16914 = FACE_OUTER_BOUND ( 'NONE', #14692, .T. ) ;
#16915 = CARTESIAN_POINT ( 'NONE',  ( 40.31606138205700063, 8.691238522346997897, 68.80501292736998664 ) ) ;
#16916 = VERTEX_POINT ( 'NONE', #7538 ) ;
#16917 = DIRECTION ( 'NONE',  ( -1.000000000000000000, 0.000000000000000000, 0.000000000000000000 ) ) ;
#16918 = DIRECTION ( 'NONE',  ( -1.000000000000000000, -1.185941393278724777E-16, -8.240782279085522416E-17 ) ) ;
#16919 = EDGE_CURVE ( 'NONE', #16043, #10464, #13084, .T. ) ;
#16920 = CARTESIAN_POINT ( 'NONE',  ( 39.38009889167648936, -11.40384086642190908, 70.00779233799264034 ) ) ;
#16921 = CARTESIAN_POINT ( 'NONE',  ( 0.000000000000000000, 0.000000000000000000, 0.000000000000000000 ) ) ;
#16922 = CARTESIAN_POINT ( 'NONE',  ( 32.56606138205700773, 43.35512946304240245, 83.12823623207320622 ) ) ;
#16923 = CARTESIAN_POINT ( 'NONE',  ( 37.25202387243752611, -25.21368208888610241, 70.00779233799262613 ) ) ;
#16924 = DIRECTION ( 'NONE',  ( 0.000000000000000000, -3.469446951953613400E-15, -1.000000000000000000 ) ) ;
#16925 = AXIS2_PLACEMENT_3D ( 'NONE', #7570, #25438, #15419 ) ;
#16926 = CARTESIAN_POINT ( 'NONE',  ( 38.37017380507018771, -27.60384086642191193, 69.64448340153876416 ) ) ;
#16927 = CARTESIAN_POINT ( 'NONE',  ( 39.75145154291258365, -29.60384086642190837, 69.64448340153876416 ) ) ;
#16928 = CARTESIAN_POINT ( 'NONE',  ( 39.29254315202756231, -22.81368208888610027, 69.94417936956672577 ) ) ;
#16929 = VERTEX_POINT ( 'NONE', #13454 ) ;
#16930 = ORIENTED_EDGE ( 'NONE', *, *, #22175, .T. ) ;
#16931 = LINE ( 'NONE', #15244, #22208 ) ;
#16932 = DIRECTION ( 'NONE',  ( 1.000000000000000000, 0.000000000000000000, 0.000000000000000000 ) ) ;
#16933 = CARTESIAN_POINT ( 'NONE',  ( 39.51027997493896748, -0.5136820888861012291, 71.32335560751961623 ) ) ;
#16934 = VERTEX_POINT ( 'NONE', #19755 ) ;
#16935 = EDGE_LOOP ( 'NONE', ( #24049, #9846, #9867, #17952 ) ) ;
#16936 = DIRECTION ( 'NONE',  ( 2.792262043613788930E-15, -0.8967398287344627850, -0.4425581086832399147 ) ) ;
#16937 = CARTESIAN_POINT ( 'NONE',  ( 43.31606138205700063, 3.973594872748516416, 6.337251443159059860 ) ) ;
#16938 = ORIENTED_EDGE ( 'NONE', *, *, #14937, .F. ) ;
#16939 = CARTESIAN_POINT ( 'NONE',  ( 43.31606138205700063, -16.48551471403133206, 77.11349248448009064 ) ) ;
#16940 = CARTESIAN_POINT ( 'NONE',  ( 38.93415946300896024, -7.503840866421907840, 69.66206559358663242 ) ) ;
#16941 = DIRECTION ( 'NONE',  ( -1.000000000000000000, 0.000000000000000000, 0.000000000000000000 ) ) ;
#16942 = CARTESIAN_POINT ( 'NONE',  ( 32.81606138205700773, 41.44123852234597649, 67.80501292736988717 ) ) ;
#16943 = VERTEX_POINT ( 'NONE', #37 ) ;
#16944 = AXIS2_PLACEMENT_3D ( 'NONE', #22124, #10287, #18278 ) ;
#16945 = ORIENTED_EDGE ( 'NONE', *, *, #8620, .T. ) ;
#16946 = ORIENTED_EDGE ( 'NONE', *, *, #11241, .T. ) ;
#16947 = CARTESIAN_POINT ( 'NONE',  ( 35.64099152588523367, -8.607181138186998481, 93.30501292736998664 ) ) ;
#16948 = CARTESIAN_POINT ( 'NONE',  ( 39.29254315202756231, 1.186317911113898838, 69.94417936956675419 ) ) ;
#16949 = EDGE_CURVE ( 'NONE', #16232, #2876, #19621, .T. ) ;
#16950 = CARTESIAN_POINT ( 'NONE',  ( 39.75915168707251723, -24.90384086642191619, 72.49904802271737481 ) ) ;
#16951 = CARTESIAN_POINT ( 'NONE',  ( 29.71606138205695657, -23.19619402982949907, 47.16846523730000484 ) ) ;
#16952 = ORIENTED_EDGE ( 'NONE', *, *, #15800, .F. ) ;
#16953 = CARTESIAN_POINT ( 'NONE',  ( 33.80700705136447937, 3.227014435054107455, 6.369498925975481285 ) ) ;
#16954 = DIRECTION ( 'NONE',  ( 1.000000000000000000, 0.000000000000000000, 0.000000000000000000 ) ) ;
#16955 = LINE ( 'NONE', #11033, #13964 ) ;
#16956 = DIRECTION ( 'NONE',  ( 0.000000000000000000, -0.3299742535180974490, 0.9439899321577398528 ) ) ;
#16957 = AXIS2_PLACEMENT_3D ( 'NONE', #22640, #4993, #11321 ) ;
#16958 = DIRECTION ( 'NONE',  ( 6.938893903907221278E-15, -1.000000000000000000, 0.000000000000000000 ) ) ;
#16959 = ORIENTED_EDGE ( 'NONE', *, *, #10328, .T. ) ;
#16960 = ORIENTED_EDGE ( 'NONE', *, *, #15205, .T. ) ;
#16961 = AXIS2_PLACEMENT_3D ( 'NONE', #352, #16458, #16081 ) ;
#16962 = CARTESIAN_POINT ( 'NONE',  ( 41.32070064951228971, -37.35828293338759920, 83.30501292737011454 ) ) ;
#16963 = CARTESIAN_POINT ( 'NONE',  ( 43.81606138205700063, 35.95440708241085304, 61.30501292736990138 ) ) ;
#16964 = EDGE_CURVE ( 'NONE', #14611, #15633, #21583, .T. ) ;
#16965 = EDGE_CURVE ( 'NONE', #1363, #21491, #7594, .T. ) ;
#16966 = CARTESIAN_POINT ( 'NONE',  ( 38.26194895904383486, -19.01368208888609956, 70.24448340153875847 ) ) ;
#16967 = ORIENTED_EDGE ( 'NONE', *, *, #24479, .F. ) ;
#16968 = EDGE_LOOP ( 'NONE', ( #24855, #4200, #421, #17095 ) ) ;
#16969 = VECTOR ( 'NONE', #4767, 1000.000000000000227 ) ;
#16970 = FACE_OUTER_BOUND ( 'NONE', #24003, .T. ) ;
#16971 = ORIENTED_EDGE ( 'NONE', *, *, #7604, .T. ) ;
#16972 = CARTESIAN_POINT ( 'NONE',  ( 36.80608444377001121, -3.313682088886100718, 70.35351908239860563 ) ) ;
#16973 = CARTESIAN_POINT ( 'NONE',  ( 39.38009889167648936, -25.40384086642190908, 70.00779233799262613 ) ) ;
#16974 = EDGE_CURVE ( 'NONE', #3435, #16742, #17062, .T. ) ;
#16975 = ADVANCED_FACE ( 'NONE', ( #15766 ), #23624, .T. ) ;
#16976 = EDGE_CURVE ( 'NONE', #3140, #5235, #15637, .T. ) ;
#16977 = CARTESIAN_POINT ( 'NONE',  ( 41.31606138205700063, 7.043113989679085307, 66.83274420321491505 ) ) ;
#16978 = CARTESIAN_POINT ( 'NONE',  ( 38.26194895904383486, 0.9863179111139001032, 69.04448340153882668 ) ) ;
#16979 = CARTESIAN_POINT ( 'NONE',  ( 29.81606138205706813, -35.90387122078357152, 69.64117576433150703 ) ) ;
#16980 = ORIENTED_EDGE ( 'NONE', *, *, #8307, .T. ) ;
#16981 = CARTESIAN_POINT ( 'NONE',  ( 42.56606138205700063, -39.60075215179220720, 69.23691647014479145 ) ) ;
#16982 = ADVANCED_FACE ( 'NONE', ( #21310 ), #3649, .F. ) ;
#16983 = DIRECTION ( 'NONE',  ( 1.445602896647339903E-16, -1.000000000000000000, 2.999999999999999839E-15 ) ) ;
#16984 = AXIS2_PLACEMENT_3D ( 'NONE', #17235, #5897, #13759 ) ;
#16985 = CARTESIAN_POINT ( 'NONE',  ( 32.56606138205700773, 42.11769259596595560, 81.89079936499673806 ) ) ;
#16986 = DIRECTION ( 'NONE',  ( -1.000000000000000000, 1.040834085586084551E-30, 3.469446951953615175E-16 ) ) ;
#16987 = DIRECTION ( 'NONE',  ( 0.000000000000000000, 0.8191520442889929088, 0.5735764363510444941 ) ) ;
#16988 = CIRCLE ( 'NONE', #16548, 0.7500000000000006661 ) ;
#16989 = CYLINDRICAL_SURFACE ( 'NONE', #24618, 1.000000000000000888 ) ;
#16990 = CARTESIAN_POINT ( 'NONE',  ( 38.31606138205699352, 47.04446929126260102, 82.37823623207320622 ) ) ;
#16991 = EDGE_CURVE ( 'NONE', #23473, #22425, #11537, .T. ) ;
#16992 = AXIS2_PLACEMENT_3D ( 'NONE', #21224, #11705, #11323 ) ;
#16993 = FACE_OUTER_BOUND ( 'NONE', #17081, .T. ) ;
#16994 = VERTEX_POINT ( 'NONE', #21569 ) ;
#16995 = ORIENTED_EDGE ( 'NONE', *, *, #3652, .T. ) ;
#16996 = CARTESIAN_POINT ( 'NONE',  ( 38.37017380507018771, -19.60384086642191193, 69.04448340153878405 ) ) ;
#16997 = VECTOR ( 'NONE', #1699, 1000.000000000000000 ) ;
#16998 = PLANE ( 'NONE',  #2540 ) ;
#16999 = CARTESIAN_POINT ( 'NONE',  ( 38.93415946300897446, -20.11368208888610809, 73.09843995877329803 ) ) ;
#17000 = LINE ( 'NONE', #25175, #4969 ) ;
#17001 = FILL_AREA_STYLE_COLOUR ( '', #16396 ) ;
#17002 = ORIENTED_EDGE ( 'NONE', *, *, #24940, .T. ) ;
#17003 = LINE ( 'NONE', #20480, #5575 ) ;
#17004 = CARTESIAN_POINT ( 'NONE',  ( 47.81606138205695089, -23.19619402982945644, 47.16846523730003327 ) ) ;
#17005 = VECTOR ( 'NONE', #14221, 1000.000000000000000 ) ;
#17006 = CARTESIAN_POINT ( 'NONE',  ( 39.02088643472237095, -24.91368208888610170, 69.02690120949091579 ) ) ;
#17007 = VERTEX_POINT ( 'NONE', #9607 ) ;
#17008 = CARTESIAN_POINT ( 'NONE',  ( 33.56606138205700773, -34.55876147765400219, 75.30501292737011454 ) ) ;
#17009 = CARTESIAN_POINT ( 'NONE',  ( 39.31606138205700063, 15.19123852234700500, 71.30501292736995822 ) ) ;
#17010 = CARTESIAN_POINT ( 'NONE',  ( 37.69796330110504101, -1.113682088886101207, 69.66206559358663242 ) ) ;
#17011 = DIRECTION ( 'NONE',  ( -1.734723475976814737E-16, 1.000000000000000000, -3.491481338843135327E-15 ) ) ;
#17012 = CIRCLE ( 'NONE', #1782, 1.750000000000001554 ) ;
#17013 = CARTESIAN_POINT ( 'NONE',  ( 37.69796330110504101, -11.11368208888610276, 69.66206559358664663 ) ) ;
#17014 = STYLED_ITEM ( 'NONE', ( #7461 ), #15967 ) ;
#17015 = DIRECTION ( 'NONE',  ( -3.717264591378870232E-16, -2.999999999999999839E-15, -1.000000000000000000 ) ) ;
#17016 = CIRCLE ( 'NONE', #943, 0.5000000000000004441 ) ;
#17017 = CARTESIAN_POINT ( 'NONE',  ( 38.26194895904384907, 1.396159133578083633, 73.11602215082119471 ) ) ;
#17018 = CARTESIAN_POINT ( 'NONE',  ( 37.21915885897815457, -18.20384086642190979, 71.67976084211552745 ) ) ;
#17019 = CARTESIAN_POINT ( 'NONE',  ( 37.33957961208646736, -3.813682088886109156, 72.81632618279323310 ) ) ;
#17020 = VERTEX_POINT ( 'NONE', #17456 ) ;
#17021 = CARTESIAN_POINT ( 'NONE',  ( 43.81606138205700063, -35.70002751211045933, 71.94742330197156832 ) ) ;
#17022 = EDGE_CURVE ( 'NONE', #8670, #23228, #22805, .T. ) ;
#17023 = VECTOR ( 'NONE', #10734, 1000.000000000000000 ) ;
#17024 = EDGE_LOOP ( 'NONE', ( #2377, #7162, #11843, #19590, #15555, #4415, #13697, #3990, #16627, #24309 ) ) ;
#17025 = CARTESIAN_POINT ( 'NONE',  ( 39.98359781491296161, -3.203840866421912903, 70.89533451361947414 ) ) ;
#17026 = CARTESIAN_POINT ( 'NONE',  ( 43.31606138205700063, -12.97731741051367393, 21.08248588348817876 ) ) ;
#17027 = AXIS2_PLACEMENT_3D ( 'NONE', #1056, #24112, #2725 ) ;
#17028 = CARTESIAN_POINT ( 'NONE',  ( 37.80618814713140097, -1.913682088886106136, 73.13360434286904876 ) ) ;
#17029 = ORIENTED_EDGE ( 'NONE', *, *, #15854, .F. ) ;
#17030 = CARTESIAN_POINT ( 'NONE',  ( 36.89935272106204422, -9.213682088886100630, 69.52238214136768590 ) ) ;
#17031 = ORIENTED_EDGE ( 'NONE', *, *, #8479, .T. ) ;
#17032 = DIRECTION ( 'NONE',  ( 0.000000000000000000, 0.7540134720837716742, 0.6568589528324746407 ) ) ;
#17033 = CARTESIAN_POINT ( 'NONE',  ( 38.73920764526923932, -5.503840866421911393, 70.26206559358664094 ) ) ;
#17034 =( GEOMETRIC_REPRESENTATION_CONTEXT ( 3 ) GLOBAL_UNCERTAINTY_ASSIGNED_CONTEXT ( ( #16730 ) ) GLOBAL_UNIT_ASSIGNED_CONTEXT ( ( #11026, #22869, #8237 ) ) REPRESENTATION_CONTEXT ( 'NONE', 'WORKASPACE' ) );
#17035 = ORIENTED_EDGE ( 'NONE', *, *, #10520, .T. ) ;
#17036 = ORIENTED_EDGE ( 'NONE', *, *, #16782, .T. ) ;
#17037 = FACE_BOUND ( 'NONE', #13015, .T. ) ;
#17038 = DIRECTION ( 'NONE',  ( 1.000000000000000000, 0.000000000000000000, 0.000000000000000000 ) ) ;
#17039 = CARTESIAN_POINT ( 'NONE',  ( 40.33642880535521869, -19.30384086642191477, 69.98269868914866265 ) ) ;
#17040 = CIRCLE ( 'NONE', #12530, 0.5000000000000004441 ) ;
#17041 = CARTESIAN_POINT ( 'NONE',  ( 36.32862050049384806, -20.47969909242301156, 75.45699727914595201 ) ) ;
#17042 = CARTESIAN_POINT ( 'NONE',  ( 36.31606138205700773, -20.93502329652820038, 27.89939821807130826 ) ) ;
#17043 = CARTESIAN_POINT ( 'NONE',  ( 39.75915168707250302, -18.71368208888610241, 70.26145752964251301 ) ) ;
#17044 = LINE ( 'NONE', #7248, #14196 ) ;
#17045 = MECHANICAL_DESIGN_GEOMETRIC_PRESENTATION_REPRESENTATION (  '', ( #4700 ), #24004 ) ;
#17046 = CARTESIAN_POINT ( 'NONE',  ( 43.81606138205700063, 45.92314894770293421, 79.37823623207320622 ) ) ;
#17047 = ORIENTED_EDGE ( 'NONE', *, *, #13211, .T. ) ;
#17048 = LINE ( 'NONE', #9676, #22775 ) ;
#17049 = FACE_OUTER_BOUND ( 'NONE', #7752, .T. ) ;
#17050 = CARTESIAN_POINT ( 'NONE',  ( 38.37017380507018771, -11.60384086642190660, 69.64448340153879258 ) ) ;
#17051 = APPLICATION_PROTOCOL_DEFINITION ( 'draft international standard', 'automotive_design', 1998, #22302 ) ;
#17052 = EDGE_CURVE ( 'NONE', #19510, #16406, #5721, .T. ) ;
#17053 = DIRECTION ( 'NONE',  ( 0.000000000000000000, 0.5706330172266920187, -0.8212051873014210024 ) ) ;
#17054 = CARTESIAN_POINT ( 'NONE',  ( 39.38009889167650357, -24.21368208888610596, 72.75271321436730432 ) ) ;
#17055 = APPLICATION_CONTEXT ( 'automotive_design' ) ;
#17056 = EDGE_CURVE ( 'NONE', #3232, #8101, #588, .T. ) ;
#17057 = PRODUCT_DEFINITION_FORMATION_WITH_SPECIFIED_SOURCE ( 'ANY', '', #9935, .NOT_KNOWN. ) ;
#17058 = CARTESIAN_POINT ( 'NONE',  ( 46.81606138205707879, -38.42645682328033274, 63.90656833300437256 ) ) ;
#17059 = EDGE_CURVE ( 'NONE', #14925, #13947, #25406, .T. ) ;
#17060 = CARTESIAN_POINT ( 'NONE',  ( 38.26194895904384907, -26.60384086642191548, 73.11602215082115208 ) ) ;
#17061 = CARTESIAN_POINT ( 'NONE',  ( 36.36697178183959522, -6.685332804587225120, 83.20286675510105567 ) ) ;
#17062 = CIRCLE ( 'NONE', #9663, 0.7500000000000031086 ) ;
#17063 = CARTESIAN_POINT ( 'NONE',  ( 38.37017380507020192, -18.01368208888611022, 73.11602215082116629 ) ) ;
#17064 = VERTEX_POINT ( 'NONE', #8548 ) ;
#17065 = CARTESIAN_POINT ( 'NONE',  ( 39.64521430340305841, -0.8038408664219169886, 73.30173637941818754 ) ) ;
#17066 = ORIENTED_EDGE ( 'NONE', *, *, #16655, .F. ) ;
#17067 = CARTESIAN_POINT ( 'NONE',  ( 31.81606138205700418, -26.97987052895604876, 80.55501292737007191 ) ) ;
#17068 = DIRECTION ( 'NONE',  ( 0.000000000000000000, 1.000000000000000000, 0.000000000000000000 ) ) ;
#17069 = CARTESIAN_POINT ( 'NONE',  ( 38.73920764526923932, -29.50384086642191050, 70.26206559358661252 ) ) ;
#17070 = ORIENTED_EDGE ( 'NONE', *, *, #6581, .F. ) ;
#17071 = ORIENTED_EDGE ( 'NONE', *, *, #24179, .T. ) ;
#17072 = CARTESIAN_POINT ( 'NONE',  ( 33.31606138205700773, 7.283211578144648257, 66.04722806671131252 ) ) ;
#17073 = ADVANCED_FACE ( 'NONE', ( #6231 ), #12172, .T. ) ;
#17074 = CARTESIAN_POINT ( 'NONE',  ( 32.81606138205700773, 41.44123852234599781, 75.30501292736987295 ) ) ;
#17075 = ORIENTED_EDGE ( 'NONE', *, *, #24985, .T. ) ;
#17076 =( NAMED_UNIT ( * ) PLANE_ANGLE_UNIT ( ) SI_UNIT ( $, .RADIAN. ) );
#17077 = CARTESIAN_POINT ( 'NONE',  ( 39.82603832034400426, -3.303840866421908995, 70.35351908239857721 ) ) ;
#17078 = CARTESIAN_POINT ( 'NONE',  ( 33.56606138205700773, 42.19123852234599781, 74.30501292736987295 ) ) ;
#17079 = CARTESIAN_POINT ( 'NONE',  ( 33.56606138205700773, 43.19123852234595518, 61.30501292736988006 ) ) ;
#17080 = VECTOR ( 'NONE', #11756, 1000.000000000000000 ) ;
#17081 = EDGE_LOOP ( 'NONE', ( #6979, #3430, #41, #13261 ) ) ;
#17082 = ORIENTED_EDGE ( 'NONE', *, *, #13429, .T. ) ;
#17083 = CARTESIAN_POINT ( 'NONE',  ( 31.81606138205700418, -30.95005513552129983, 81.04249030099066431 ) ) ;
#17084 = CARTESIAN_POINT ( 'NONE',  ( 37.80618814713140097, 0.08631791111389161553, 73.13360434286904876 ) ) ;
#17085 = VERTEX_POINT ( 'NONE', #10485 ) ;
#17086 = CARTESIAN_POINT ( 'NONE',  ( 39.75915168707251723, -28.90384086642191619, 72.49904802271737481 ) ) ;
#17087 = CARTESIAN_POINT ( 'NONE',  ( 43.31606138205700063, -27.60498114914042134, 57.04949906928994352 ) ) ;
#17088 = VERTEX_POINT ( 'NONE', #792 ) ;
#17089 = LINE ( 'NONE', #24907, #13136 ) ;
#17090 = CARTESIAN_POINT ( 'NONE',  ( 34.81606138205696510, -0.8482369431493941292, -3.067843137301039302 ) ) ;
#17091 = CARTESIAN_POINT ( 'NONE',  ( 30.81606138205700418, 40.39281886181299797, 66.30501292737000085 ) ) ;
#17092 =( NAMED_UNIT ( * ) SI_UNIT ( $, .STERADIAN. ) SOLID_ANGLE_UNIT ( ) );
#17093 = ORIENTED_EDGE ( 'NONE', *, *, #978, .T. ) ;
#17094 = DIRECTION ( 'NONE',  ( 1.000000000000000000, 2.751104698760144965E-15, -1.228345504986737969E-16 ) ) ;
#17095 = ORIENTED_EDGE ( 'NONE', *, *, #9151, .T. ) ;
#17096 = ORIENTED_EDGE ( 'NONE', *, *, #7196, .T. ) ;
#17097 = AXIS2_PLACEMENT_3D ( 'NONE', #14934, #3203, #22665 ) ;
#17098 = LINE ( 'NONE', #20704, #23534 ) ;
#17099 = LINE ( 'NONE', #10918, #25486 ) ;
#17100 = CARTESIAN_POINT ( 'NONE',  ( 38.26194895904383486, -15.01368208888610134, 70.24448340153875847 ) ) ;
#17101 = EDGE_LOOP ( 'NONE', ( #6884, #3164, #10254, #23165 ) ) ;
#17102 = ORIENTED_EDGE ( 'NONE', *, *, #20979, .T. ) ;
#17103 = EDGE_CURVE ( 'NONE', #20448, #18554, #5955, .T. ) ;
#17104 = DIRECTION ( 'NONE',  ( 1.000000000000000000, 2.751104698760144965E-15, -1.228345504986737969E-16 ) ) ;
#17105 = VERTEX_POINT ( 'NONE', #12424 ) ;
#17106 = DIRECTION ( 'NONE',  ( 1.000000000000000000, 2.999999999999999839E-15, 0.000000000000000000 ) ) ;
#17107 = CARTESIAN_POINT ( 'NONE',  ( 38.93415946300896024, -25.50384086642190340, 69.66206559358660400 ) ) ;
#17108 = CARTESIAN_POINT ( 'NONE',  ( 40.64099152588522657, -9.607181138187000258, 80.05501292737000085 ) ) ;
#17109 = CARTESIAN_POINT ( 'NONE',  ( 36.29569395875879678, -1.313682088886099830, 69.98269868914869107 ) ) ;
#17110 = VERTEX_POINT ( 'NONE', #16263 ) ;
#17111 = DIRECTION ( 'NONE',  ( -0.000000000000000000, -1.000000000000000000, 2.999999999999998655E-15 ) ) ;
#17112 = DIRECTION ( 'NONE',  ( 1.000000000000000000, -0.000000000000000000, 0.000000000000000000 ) ) ;
#17113 = LINE ( 'NONE', #3057, #16137 ) ;
#17114 = ADVANCED_FACE ( 'NONE', ( #18339 ), #4559, .F. ) ;
#17115 = ADVANCED_FACE ( 'NONE', ( #20263 ), #22445, .T. ) ;
#17116 = CARTESIAN_POINT ( 'NONE',  ( 40.11623881305710881, -6.323019409765026744, 83.24594533976426192 ) ) ;
#17117 = DIRECTION ( 'NONE',  ( 5.047295537021760406E-31, -1.000000000000000000, 3.491481338843135327E-15 ) ) ;
#17118 = B_SPLINE_SURFACE_WITH_KNOTS ( 'NONE', 1, 3, ( 
 ( #21285, #9331, #7765, #17175, #15104, #13061 ),
 ( #5326, #25124, #15231, #3628, #17428, #7641 ),
 ( #15483, #23331, #13188, #25383, #5697, #13561 ),
 ( #17304, #13316, #15609, #7506, #11640, #15358 ) ),
 .UNSPECIFIED., .F., .F., .F.,
 ( 2, 1, 1, 2 ),
 ( 4, 2, 4 ),
 ( -0.01000000000000000021, 0.000000000000000000, 1.000000000000000000, 1.010099999999999998 ),
 ( 0.000000000000000000, 0.5000000000000000000, 1.000000000000000000 ),
 .UNSPECIFIED. ) ;
#17119 = LINE ( 'NONE', #19415, #5327 ) ;
#17120 = EDGE_CURVE ( 'NONE', #7648, #7039, #16134, .T. ) ;
#17121 = ORIENTED_EDGE ( 'NONE', *, *, #8809, .T. ) ;
#17122 = FACE_OUTER_BOUND ( 'NONE', #25173, .T. ) ;
#17123 = LINE ( 'NONE', #12877, #24282 ) ;
#17124 = VERTEX_POINT ( 'NONE', #8425 ) ;
#17125 = ORIENTED_EDGE ( 'NONE', *, *, #3339, .F. ) ;
#17126 = CARTESIAN_POINT ( 'NONE',  ( 38.26194895904384197, -10.60384086642192081, 73.71602215082116061 ) ) ;
#17127 = EDGE_CURVE ( 'NONE', #2353, #18040, #20140, .T. ) ;
#17128 = DIRECTION ( 'NONE',  ( 0.000000000000000000, 1.000000000000000000, -2.999999999999999839E-15 ) ) ;
#17129 = CARTESIAN_POINT ( 'NONE',  ( 39.98359781491296161, -16.41368208888610525, 71.86517103874047052 ) ) ;
#17130 = ORIENTED_EDGE ( 'NONE', *, *, #5951, .F. ) ;
#17131 = CARTESIAN_POINT ( 'NONE',  ( 46.81606138205697221, -5.022037326221683529, -5.474317061061731771 ) ) ;
#17132 = CARTESIAN_POINT ( 'NONE',  ( 36.31606138205702194, -19.68901644060773037, 25.93955620509758475 ) ) ;
#17133 = CARTESIAN_POINT ( 'NONE',  ( 39.64521430340304420, -18.81368208888610027, 69.45876917294175712 ) ) ;
#17134 = ORIENTED_EDGE ( 'NONE', *, *, #18913, .F. ) ;
#17135 =( NAMED_UNIT ( * ) SI_UNIT ( $, .STERADIAN. ) SOLID_ANGLE_UNIT ( ) );
#17136 = LINE ( 'NONE', #7342, #20540 ) ;
#17137 = LINE ( 'NONE', #5281, #19496 ) ;
#17138 = EDGE_CURVE ( 'NONE', #12100, #17728, #14088, .T. ) ;
#17139 = CARTESIAN_POINT ( 'NONE',  ( 33.56606138205700773, 41.44123852234599781, 74.30501292736987295 ) ) ;
#17140 = LINE ( 'NONE', #24718, #10457 ) ;
#17141 = EDGE_CURVE ( 'NONE', #8838, #16943, #6481, .T. ) ;
#17142 = CARTESIAN_POINT ( 'NONE',  ( 37.60469502381300799, -16.40384086642191264, 72.26730301774234988 ) ) ;
#17143 = CARTESIAN_POINT ( 'NONE',  ( 39.38009889167650357, 1.786317911113891821, 72.75271321436734695 ) ) ;
#17144 = ADVANCED_FACE ( 'NONE', ( #10105 ), #2228, .F. ) ;
#17145 = ORIENTED_EDGE ( 'NONE', *, *, #12501, .F. ) ;
#17146 = CARTESIAN_POINT ( 'NONE',  ( 31.81606138205700418, -3.831401139557048197, 80.75501292737000369 ) ) ;
#17147 = PLANE ( 'NONE',  #10293 ) ;
#17148 = ORIENTED_EDGE ( 'NONE', *, *, #6149, .F. ) ;
#17149 = ORIENTED_EDGE ( 'NONE', *, *, #7059, .T. ) ;
#17150 = CARTESIAN_POINT ( 'NONE',  ( 37.69796330110505522, -0.5038408664219152788, 73.09843995877331224 ) ) ;
#17151 = ADVANCED_FACE ( 'NONE', ( #2720 ), #22320, .T. ) ;
#17152 = CARTESIAN_POINT ( 'NONE',  ( 36.49096545463212493, 0.4863179111138959954, 71.43714994484035685 ) ) ;
#17153 = CARTESIAN_POINT ( 'NONE',  ( 40.26954217208371034, -10.71368208888610063, 69.89063713639259845 ) ) ;
#17154 = EDGE_LOOP ( 'NONE', ( #9148, #12711, #10153, #7018 ) ) ;
#17155 = CARTESIAN_POINT ( 'NONE',  ( 37.31606138205700063, 43.19123852234595518, 61.30501292736988006 ) ) ;
#17156 = VECTOR ( 'NONE', #24519, 1000.000000000000000 ) ;
#17157 = CARTESIAN_POINT ( 'NONE',  ( 39.37952058850012804, -3.003840866421910505, 71.78268878715392987 ) ) ;
#17158 = AXIS2_PLACEMENT_3D ( 'NONE', #17421, #22955, #11506 ) ;
#17159 = VECTOR ( 'NONE', #14450, 1000.000000000000000 ) ;
#17160 = CARTESIAN_POINT ( 'NONE',  ( 40.31606138205700773, -26.06829118875199214, 77.52306850662461102 ) ) ;
#17161 = VERTEX_POINT ( 'NONE', #4679 ) ;
#17162 = DIRECTION ( 'NONE',  ( 9.027796614315171564E-31, 1.000000000000000000, 3.938893903907230117E-15 ) ) ;
#17163 = DIRECTION ( 'NONE',  ( 0.000000000000000000, -0.6568589528324746407, 0.7540134720837716742 ) ) ;
#17164 = CARTESIAN_POINT ( 'NONE',  ( 39.73277004305197124, -7.403840866421910860, 69.52238214136768590 ) ) ;
#17165 = CARTESIAN_POINT ( 'NONE',  ( 38.05466885408097255, -22.20850315994778867, 75.29993782803930458 ) ) ;
#17166 = DIRECTION ( 'NONE',  ( 1.000000000000000000, 0.000000000000000000, -0.000000000000000000 ) ) ;
#17167 = CARTESIAN_POINT ( 'NONE',  ( 39.29254315202756231, -20.81368208888610027, 69.94417936956672577 ) ) ;
#17168 = DIRECTION ( 'NONE',  ( -1.000000000000000000, -1.950367120401949903E-17, 2.478176394252580155E-16 ) ) ;
#17169 = EDGE_CURVE ( 'NONE', #12037, #25254, #412, .T. ) ;
#17170 = CARTESIAN_POINT ( 'NONE',  ( 43.31606138205700063, 3.172506336381830661, 12.50058896911730066 ) ) ;
#17171 = VERTEX_POINT ( 'NONE', #24361 ) ;
#17172 = LINE ( 'NONE', #13556, #22518 ) ;
#17173 = CARTESIAN_POINT ( 'NONE',  ( 39.98359781491296161, -9.203840866421911571, 70.89533451361947414 ) ) ;
#17174 = APPLICATION_PROTOCOL_DEFINITION ( 'draft international standard', 'automotive_design', 1998, #396 ) ;
#17175 = CARTESIAN_POINT ( 'NONE',  ( 32.99125882899717510, 3.408086086664901870, 6.165992285920837368 ) ) ;
#17176 = CARTESIAN_POINT ( 'NONE',  ( 39.82603832034400426, -24.31368208888611093, 72.40698646996131060 ) ) ;
#17177 = AXIS2_PLACEMENT_3D ( 'NONE', #384, #10458, #8269 ) ;
#17178 = CIRCLE ( 'NONE', #18411, 1.000000000000000888 ) ;
#17179 = DIRECTION ( 'NONE',  ( 1.000000000000000000, -0.000000000000000000, 0.000000000000000000 ) ) ;
#17180 = CARTESIAN_POINT ( 'NONE',  ( 39.98359781491296161, -27.20384086642191335, 70.89533451361944572 ) ) ;
#17181 = LINE ( 'NONE', #25005, #12237 ) ;
#17182 = CARTESIAN_POINT ( 'NONE',  ( 36.80608444377001121, -21.31368208888610027, 70.35351908239857721 ) ) ;
#17183 = VERTEX_POINT ( 'NONE', #14589 ) ;
#17184 = CARTESIAN_POINT ( 'NONE',  ( 38.26194895904384197, -0.6038408664219181432, 73.71602215082116061 ) ) ;
#17185 = ORIENTED_EDGE ( 'NONE', *, *, #717, .F. ) ;
#17186 = DIRECTION ( 'NONE',  ( -1.000000000000000000, -2.156013462999745228E-15, 0.000000000000000000 ) ) ;
#17187 = CARTESIAN_POINT ( 'NONE',  ( 32.56606138205700773, -26.74044063519535186, 82.55501292737007191 ) ) ;
#17188 = CARTESIAN_POINT ( 'NONE',  ( 37.69225076346193504, -25.80384086642191477, 70.42958956619166599 ) ) ;
#17189 = ORIENTED_EDGE ( 'NONE', *, *, #9290, .T. ) ;
#17190 = ORIENTED_EDGE ( 'NONE', *, *, #13816, .F. ) ;
#17191 = CARTESIAN_POINT ( 'NONE',  ( 31.81606138205700418, -26.74044063519535186, 82.50501292737007475 ) ) ;
#17192 = CARTESIAN_POINT ( 'NONE',  ( 43.82106138205700319, 4.103895195095678794, 6.341006091748962348 ) ) ;
#17193 = ORIENTED_EDGE ( 'NONE', *, *, #8147, .F. ) ;
#17194 = LINE ( 'NONE', #23104, #7771 ) ;
#17195 = CARTESIAN_POINT ( 'NONE',  ( 37.25202387243754032, -6.403840866421914413, 72.75271321436733274 ) ) ;
#17196 = EDGE_CURVE ( 'NONE', #24226, #18636, #15235, .T. ) ;
#17197 = ADVANCED_FACE ( 'NONE', ( #8167 ), #10227, .F. ) ;
#17198 = TOROIDAL_SURFACE ( 'NONE', #9388, 1.800000000000000044, 0.2000000000000000111 ) ;
#17199 = AXIS2_PLACEMENT_3D ( 'NONE', #3026, #8591, #2764 ) ;
#17200 = CARTESIAN_POINT ( 'NONE',  ( 42.96606138205698500, -6.672912525257881811, -0.4345143786933236552 ) ) ;
#17201 = DIRECTION ( 'NONE',  ( 2.312964634635742267E-15, -0.8967398287344634511, -0.4425581086832385824 ) ) ;
#17202 = VERTEX_POINT ( 'NONE', #2476 ) ;
#17203 = ORIENTED_EDGE ( 'NONE', *, *, #19452, .T. ) ;
#17204 = DIRECTION ( 'NONE',  ( 0.000000000000000000, -1.000000000000000000, 3.965082230804126670E-15 ) ) ;
#17205 = CARTESIAN_POINT ( 'NONE',  ( 37.33957961208646736, -1.813682088886107380, 72.81632618279323310 ) ) ;
#17206 = MANIFOLD_SOLID_BREP ( 'Stock-MAS-155-1', #13081 ) ;
#17207 = LINE ( 'NONE', #20943, #13104 ) ;
#17208 = CARTESIAN_POINT ( 'NONE',  ( 44.81606138205700063, 41.44123852234599781, 75.30501292736987295 ) ) ;
#17209 = ORIENTED_EDGE ( 'NONE', *, *, #15933, .T. ) ;
#17210 = DIRECTION ( 'NONE',  ( 3.614007241618344826E-17, -1.000000000000000000, 2.999999999999999839E-15 ) ) ;
#17211 = EDGE_CURVE ( 'NONE', #9789, #13993, #2533, .T. ) ;
#17212 = AXIS2_PLACEMENT_3D ( 'NONE', #24286, #7173, #16956 ) ;
#17213 = PLANE ( 'NONE',  #6155 ) ;
#17214 = CARTESIAN_POINT ( 'NONE',  ( 37.14448850680319936, -22.27515649656511698, 29.48506754039016542 ) ) ;
#17215 = SHAPE_REPRESENTATION_RELATIONSHIP ( 'NONE' , 'NONE' ,  #10266, #6130 ) ;
#17216 = VERTEX_POINT ( 'NONE', #3115 ) ;
#17217 = AXIS2_PLACEMENT_3D ( 'NONE', #4933, #10989, #24872 ) ;
#17218 = AXIS2_PLACEMENT_3D ( 'NONE', #16559, #22240, #2766 ) ;
#17219 = DIRECTION ( 'NONE',  ( 1.734723475976814737E-16, -1.000000000000000000, 3.491481338843135327E-15 ) ) ;
#17220 = ORIENTED_EDGE ( 'NONE', *, *, #22176, .T. ) ;
#17221 = EDGE_LOOP ( 'NONE', ( #11542, #15090, #2746, #13366 ) ) ;
#17222 = DIRECTION ( 'NONE',  ( -1.000000000000000000, 6.018531076210110289E-31, 1.734723475976804876E-16 ) ) ;
#17223 = CARTESIAN_POINT ( 'NONE',  ( 38.37017380507020192, -10.01368208888610312, 72.51602215082118619 ) ) ;
#17224 = CARTESIAN_POINT ( 'NONE',  ( 37.69225076346193504, -9.813682088886100274, 72.33091598616827866 ) ) ;
#17225 = VERTEX_POINT ( 'NONE', #7377 ) ;
#17226 = EDGE_LOOP ( 'NONE', ( #5408, #1888, #21772, #23043 ) ) ;
#17227 = CYLINDRICAL_SURFACE ( 'NONE', #14096, 1.750000000000001554 ) ;
#17228 = CARTESIAN_POINT ( 'NONE',  ( 39.82603832034400426, 1.686317911113891732, 72.40698646996136745 ) ) ;
#17229 = CARTESIAN_POINT ( 'NONE',  ( 36.49096545463212493, -22.10384086642191548, 71.32335560751961623 ) ) ;
#17230 = MECHANICAL_DESIGN_GEOMETRIC_PRESENTATION_REPRESENTATION (  '', ( #20939 ), #21339 ) ;
#17231 = CARTESIAN_POINT ( 'NONE',  ( 42.74055771317608787, 3.188265934946779012, 6.371314334530746137 ) ) ;
#17232 = AXIS2_PLACEMENT_3D ( 'NONE', #17974, #6242, #8308 ) ;
#17233 = CARTESIAN_POINT ( 'NONE',  ( 35.91606138205695231, 2.926944320371551278, 0.2449088955976189141 ) ) ;
#17234 = DIRECTION ( 'NONE',  ( 1.734723475976814737E-16, -1.000000000000000000, 3.491481338843135327E-15 ) ) ;
#17235 = CARTESIAN_POINT ( 'NONE',  ( 32.81606138205700773, 45.92314894770293421, 80.37823623207322044 ) ) ;
#17236 = DIRECTION ( 'NONE',  ( 0.000000000000000000, 2.775557561562888984E-15, 1.000000000000000000 ) ) ;
#17237 = CARTESIAN_POINT ( 'NONE',  ( 33.31606138205700773, -10.93995761290683255, 80.99653337025984001 ) ) ;
#17238 = ADVANCED_FACE ( 'NONE', ( #12674 ), #2849, .F. ) ;
#17239 = VECTOR ( 'NONE', #4253, 1000.000000000000000 ) ;
#17240 = CARTESIAN_POINT ( 'NONE',  ( 35.31606138205700773, 3.043703737701412226, 64.67489359404071081 ) ) ;
#17241 = ORIENTED_EDGE ( 'NONE', *, *, #24414, .T. ) ;
#17242 = CARTESIAN_POINT ( 'NONE',  ( 35.31606138205687273, 43.19123852234596939, 65.30501292736988717 ) ) ;
#17243 = MANIFOLD_SOLID_BREP ( 'Stock-MAS-155-1', #16754 ) ;
#17244 = LINE ( 'NONE', #21234, #2872 ) ;
#17245 = ORIENTED_EDGE ( 'NONE', *, *, #12563, .T. ) ;
#17246 = ORIENTED_EDGE ( 'NONE', *, *, #14386, .F. ) ;
#17247 = CARTESIAN_POINT ( 'NONE',  ( 37.61123632939164452, -13.70384086642191157, 69.02690120949091579 ) ) ;
#17248 = AXIS2_PLACEMENT_3D ( 'NONE', #20242, #12536, #12402 ) ;
#17249 = CARTESIAN_POINT ( 'NONE',  ( 46.81606138205695800, -0.2703287878657641974, 1.505452687840413972 ) ) ;
#17250 = CARTESIAN_POINT ( 'NONE',  ( 37.69796330110504101, -15.11368208888609743, 69.66206559358661821 ) ) ;
#17251 = CIRCLE ( 'NONE', #7806, 2.500000000000002220 ) ;
#17252 = EDGE_LOOP ( 'NONE', ( #24785, #7776, #22316, #14890, #8280 ) ) ;
#17253 = DIRECTION ( 'NONE',  ( 0.000000000000000000, -3.225463739888140187E-15, -1.000000000000000000 ) ) ;
#17254 = LINE ( 'NONE', #22913, #12111 ) ;
#17255 = CARTESIAN_POINT ( 'NONE',  ( 40.52078840805428683, -20.61368208888610454, 70.60699637195608602 ) ) ;
#17256 = VERTEX_POINT ( 'NONE', #3238 ) ;
#17257 = CIRCLE ( 'NONE', #24236, 1.499999999999999778 ) ;
#17258 = FACE_BOUND ( 'NONE', #17252, .T. ) ;
#17259 = CARTESIAN_POINT ( 'NONE',  ( 30.81606138205706102, -34.13844651005150155, 70.48338531520533934 ) ) ;
#17260 = CYLINDRICAL_SURFACE ( 'NONE', #12469, 1.750000000000001554 ) ;
#17261 = AXIS2_PLACEMENT_3D ( 'NONE', #15302, #22781, #20852 ) ;
#17262 = DIRECTION ( 'NONE',  ( 0.000000000000000000, 0.7540134720837716742, 0.6568589528324746407 ) ) ;
#17263 = EDGE_CURVE ( 'NONE', #5682, #16417, #10865, .T. ) ;
#17264 = LINE ( 'NONE', #5415, #23175 ) ;
#17265 = CIRCLE ( 'NONE', #11527, 10.00000000000000000 ) ;
#17266 = CARTESIAN_POINT ( 'NONE',  ( 38.63098279924290068, -10.70384086642191335, 72.53360434286905445 ) ) ;
#17267 = CARTESIAN_POINT ( 'NONE',  ( 39.29254315202756231, 1.186317911113898838, 69.94417936956675419 ) ) ;
#17268 = ORIENTED_EDGE ( 'NONE', *, *, #17754, .T. ) ;
#17269 = AXIS2_PLACEMENT_3D ( 'NONE', #18203, #4548, #4418 ) ;
#17270 = CARTESIAN_POINT ( 'NONE',  ( 40.31606138205700773, -19.28757846107943763, 24.56123906878952567 ) ) ;
#17271 = LINE ( 'NONE', #9930, #6171 ) ;
#17272 = EDGE_LOOP ( 'NONE', ( #4949, #17692, #7816, #6007, #8677, #11814, #1106 ) ) ;
#17273 = ORIENTED_EDGE ( 'NONE', *, *, #9003, .T. ) ;
#17274 = CIRCLE ( 'NONE', #22621, 1.499999999999999778 ) ;
#17275 = CARTESIAN_POINT ( 'NONE',  ( 36.68196826583682935, -0.003840866421911393047, 70.79240656858108593 ) ) ;
#17276 = CARTESIAN_POINT ( 'NONE',  ( 38.82593461698262871, -0.9136820888861022505, 69.62690120949091011 ) ) ;
#17277 = CARTESIAN_POINT ( 'NONE',  ( 36.36258059203031934, -5.713682088886106847, 72.86986841596736042 ) ) ;
#17278 = VECTOR ( 'NONE', #18182, 1000.000000000000000 ) ;
#17279 = EDGE_LOOP ( 'NONE', ( #11465, #25334, #19090, #12446 ) ) ;
#17280 = DIRECTION ( 'NONE',  ( 0.000000000000000000, 0.9992330079037401447, -0.03915859951075795903 ) ) ;
#17281 = CARTESIAN_POINT ( 'NONE',  ( 38.93987200065210175, -6.803840866421912104, 72.33091598616827866 ) ) ;
#17282 = EDGE_CURVE ( 'NONE', #20889, #5342, #7890, .T. ) ;
#17283 = DIRECTION ( 'NONE',  ( 1.734723475976814737E-16, -1.000000000000000000, 3.491481338843135327E-15 ) ) ;
#17284 = ADVANCED_FACE ( 'NONE', ( #5315 ), #22698, .T. ) ;
#17285 = ORIENTED_EDGE ( 'NONE', *, *, #10191, .F. ) ;
#17286 = CARTESIAN_POINT ( 'NONE',  ( 43.31606138205700063, 3.392460599465057403, 64.84545171350526971 ) ) ;
#17287 = CARTESIAN_POINT ( 'NONE',  ( 32.31606138205700063, 10.06218483883314718, 67.80501292737497465 ) ) ;
#17288 = CARTESIAN_POINT ( 'NONE',  ( 39.73277004305197124, -9.403840866421907307, 69.52238214136768590 ) ) ;
#17289 = ADVANCED_FACE ( 'NONE', ( #9068 ), #16772, .F. ) ;
#17290 = ADVANCED_FACE ( 'NONE', ( #7118 ), #6172, .T. ) ;
#17291 = EDGE_CURVE ( 'NONE', #22414, #24159, #7902, .T. ) ;
#17292 = CARTESIAN_POINT ( 'NONE',  ( 33.31606138205700773, -16.77230293220685198, 77.52306850662458260 ) ) ;
#17293 = DIRECTION ( 'NONE',  ( 1.734723475976814737E-16, -1.000000000000000000, 3.491481338843135327E-15 ) ) ;
#17294 = CARTESIAN_POINT ( 'NONE',  ( 37.33957961208646736, -15.81368208888610916, 72.81632618279321889 ) ) ;
#17295 = DIRECTION ( 'NONE',  ( -1.047880217021202589E-15, 0.4425581086832399147, -0.8967398287344627850 ) ) ;
#17296 = CIRCLE ( 'NONE', #10714, 1.750000000000001554 ) ;
#17297 = DIRECTION ( 'NONE',  ( -1.000000000000000000, 6.018531076210110289E-31, 1.734723475976804876E-16 ) ) ;
#17298 = AXIS2_PLACEMENT_3D ( 'NONE', #88, #17632, #13506 ) ;
#17299 = PLANE ( 'NONE',  #4828 ) ;
#17300 = EDGE_CURVE ( 'NONE', #21524, #21641, #19595, .T. ) ;
#17301 = CARTESIAN_POINT ( 'NONE',  ( 39.38009889167648936, -7.403840866421908196, 70.00779233799264034 ) ) ;
#17303 = EDGE_CURVE ( 'NONE', #21293, #23789, #14061, .T. ) ;
#17302 = SHAPE_DEFINITION_REPRESENTATION ( #21867, #14735 ) ;
#17304 = CARTESIAN_POINT ( 'NONE',  ( 33.32111138205700485, 4.124002793203064066, 6.312068993173404863 ) ) ;
#17305 = CARTESIAN_POINT ( 'NONE',  ( 36.49096545463212493, -15.51368208888610667, 71.43714994484034264 ) ) ;
#17306 = CARTESIAN_POINT ( 'NONE',  ( 32.81606138205700773, 41.44123852234599781, 75.30501292736987295 ) ) ;
#17307 = CARTESIAN_POINT ( 'NONE',  ( 40.14115730948191185, -21.10384086642191193, 71.43714994484030001 ) ) ;
#17308 = DIRECTION ( 'NONE',  ( -1.000000000000000000, 0.000000000000000000, 0.000000000000000000 ) ) ;
#17309 = EDGE_CURVE ( 'NONE', #24921, #22752, #15474, .T. ) ;
#17310 = CARTESIAN_POINT ( 'NONE',  ( 38.82593461698262871, -18.91368208888609459, 69.62690120949091011 ) ) ;
#17311 = ORIENTED_EDGE ( 'NONE', *, *, #6981, .F. ) ;
#17312 = CARTESIAN_POINT ( 'NONE',  ( 37.50301148336529167, -25.11368208888610454, 69.06206559358663810 ) ) ;
#17313 = ORIENTED_EDGE ( 'NONE', *, *, #18156, .T. ) ;
#17314 = LINE ( 'NONE', #13445, #9468 ) ;
#17315 = DIRECTION ( 'NONE',  ( -9.027796614315171564E-31, -1.000000000000000000, -3.938893903907230117E-15 ) ) ;
#17316 = CIRCLE ( 'NONE', #5380, 0.5000000000000000000 ) ;
#17317 = CARTESIAN_POINT ( 'NONE',  ( 37.21915885897815457, -26.20384086642190979, 71.67976084211551324 ) ) ;
#17318 = ORIENTED_EDGE ( 'NONE', *, *, #23339, .T. ) ;
#17319 = ORIENTED_EDGE ( 'NONE', *, *, #593, .T. ) ;
#17320 = CARTESIAN_POINT ( 'NONE',  ( 39.60857575084318682, -28.82472769709708516, 70.68354409430698126 ) ) ;
#17321 = CARTESIAN_POINT ( 'NONE',  ( 38.31606138205700063, 40.69123852234599781, 71.30501292737000085 ) ) ;
#17322 = ORIENTED_EDGE ( 'NONE', *, *, #6265, .F. ) ;
#17323 = CARTESIAN_POINT ( 'NONE',  ( 35.86008812008917346, -26.10384086642191903, 71.32335560751960202 ) ) ;
#17324 =( NAMED_UNIT ( * ) PLANE_ANGLE_UNIT ( ) SI_UNIT ( $, .RADIAN. ) );
#17325 = B_SPLINE_SURFACE_WITH_KNOTS ( 'NONE', 1, 3, ( 
 ( #18991, #1332, #3135, #5083 ),
 ( #8951, #25010, #7141, #9218 ) ),
 .UNSPECIFIED., .F., .F., .F.,
 ( 2, 2 ),
 ( 4, 4 ),
 ( 0.000000000000000000, 1.000000000000000000 ),
 ( 0.000000000000000000, 1.000000000000000000 ),
 .UNSPECIFIED. ) ;
#17326 = PLANE ( 'NONE',  #16363 ) ;
#17327 = EDGE_LOOP ( 'NONE', ( #15260, #3819, #2868, #21964 ) ) ;
#17328 = LINE ( 'NONE', #1348, #3017 ) ;
#17329 = DIRECTION ( 'NONE',  ( -1.734723475976814737E-16, 1.000000000000000000, -3.491481338843135327E-15 ) ) ;
#17330 = MANIFOLD_SOLID_BREP ( 'NONE', #7316 ) ;
#17331 = CARTESIAN_POINT ( 'NONE',  ( 39.38009889167648936, -25.40384086642190908, 70.00779233799262613 ) ) ;
#17332 = DIRECTION ( 'NONE',  ( 1.327674326049719602E-15, -0.4425581086832399147, 0.8967398287344627850 ) ) ;
#17333 = VECTOR ( 'NONE', #18893, 1000.000000000000227 ) ;
#17334 =( BOUNDED_CURVE ( )  B_SPLINE_CURVE ( 3, ( #24518, #9099, #3146, #4963 ),
 .UNSPECIFIED., .F., .T. ) 
 B_SPLINE_CURVE_WITH_KNOTS ( ( 4, 4 ),
 ( 1.570796326794895004, 3.141592653589795336 ),
 .UNSPECIFIED. ) 
 CURVE ( )  GEOMETRIC_REPRESENTATION_ITEM ( )  RATIONAL_B_SPLINE_CURVE ( ( 1.000000000000000000, 0.8047378541243649375, 0.8047378541243649375, 1.000000000000000000 ) ) 
 REPRESENTATION_ITEM ( '' )  );
#17335 = EDGE_LOOP ( 'NONE', ( #6625, #8289, #14880, #4037 ) ) ;
#17336 = DIRECTION ( 'NONE',  ( 1.156482317317870492E-16, 0.4425581086832399702, -0.8967398287344626739 ) ) ;
#17337 = DIRECTION ( 'NONE',  ( -0.000000000000000000, 1.000000000000000000, 0.000000000000000000 ) ) ;
#17338 = CARTESIAN_POINT ( 'NONE',  ( 40.31606138205700773, -4.357181138186154712, 72.80501292736992980 ) ) ;
#17339 = CARTESIAN_POINT ( 'NONE',  ( 37.89291511884479036, -8.503840866421912281, 72.49843995877331793 ) ) ;
#17340 = VERTEX_POINT ( 'NONE', #21276 ) ;
#17341 = PRODUCT_DEFINITION ( 'UNKNOWN', '', #4717, #25202 ) ;
#17342 = CARTESIAN_POINT ( 'NONE',  ( 43.81606138205700063, 34.92314894770294131, 80.37823623207323465 ) ) ;
#17343 = EDGE_LOOP ( 'NONE', ( #17379, #10264, #16074, #14421 ) ) ;
#17344 = ORIENTED_EDGE ( 'NONE', *, *, #422, .T. ) ;
#17345 = CARTESIAN_POINT ( 'NONE',  ( 28.81606138205695444, -23.19619402982950263, 47.16846523730000484 ) ) ;
#17346 = CARTESIAN_POINT ( 'NONE',  ( 37.38336156205274818, -13.71368208888610241, 72.12822762946750288 ) ) ;
#17347 = CARTESIAN_POINT ( 'NONE',  ( 39.24876120206128860, -12.71368208888610241, 70.63227792289245599 ) ) ;
#17348 = VERTEX_POINT ( 'NONE', #1552 ) ;
#17349 = ORIENTED_EDGE ( 'NONE', *, *, #4522, .F. ) ;
#17350 = DIRECTION ( 'NONE',  ( 0.000000000000000000, 0.6568589528324745297, -0.7540134720837717852 ) ) ;
#17351 = ORIENTED_EDGE ( 'NONE', *, *, #20305, .F. ) ;
#17352 = DIRECTION ( 'NONE',  ( -1.000000000000000000, -3.091505625455828697E-15, -4.515976121274771690E-17 ) ) ;
#17353 = CARTESIAN_POINT ( 'NONE',  ( 37.69796330110505522, -20.50384086642191050, 73.09843995877329803 ) ) ;
#17354 = CARTESIAN_POINT ( 'NONE',  ( 39.31606138205700063, 42.19123852234599781, 74.30501292736987295 ) ) ;
#17355 = COLOUR_RGB ( '', 0.08235294, 0.09019608, 0.10196078) ;
#17356 = CARTESIAN_POINT ( 'NONE',  ( 37.25260217561390874, -15.61368208888610276, 71.78268878715392987 ) ) ;
#17357 = ORIENTED_EDGE ( 'NONE', *, *, #13920, .F. ) ;
#17358 = ORIENTED_EDGE ( 'NONE', *, *, #2690, .T. ) ;
#17359 = CARTESIAN_POINT ( 'NONE',  ( 36.31606138205700063, 42.19123852234596939, 66.30501292736988717 ) ) ;
#17360 = CARTESIAN_POINT ( 'NONE',  ( 30.81606138205697576, -4.349482454670884124, -5.142398479549302515 ) ) ;
#17361 = CYLINDRICAL_SURFACE ( 'NONE', #9980, 1.000000000000000888 ) ;
#17362 = CARTESIAN_POINT ( 'NONE',  ( 38.96303889229209716, -5.307214332739725648, 83.30462760643098363 ) ) ;
#17363 = CARTESIAN_POINT ( 'NONE',  ( 44.81606138205700063, -26.97987052895604876, 80.55501292737007191 ) ) ;
#17364 = AXIS2_PLACEMENT_3D ( 'NONE', #2788, #8874, #9131 ) ;
#17365 = AXIS2_PLACEMENT_3D ( 'NONE', #14647, #8483, #24425 ) ;
#17366 = EDGE_CURVE ( 'NONE', #13895, #22610, #21158, .T. ) ;
#17367 = CARTESIAN_POINT ( 'NONE',  ( 36.31606138205700063, -26.06829118875199924, 75.30501292736998664 ) ) ;
#17368 = EDGE_CURVE ( 'NONE', #7931, #11230, #19724, .T. ) ;
#17369 = VERTEX_POINT ( 'NONE', #13803 ) ;
#17370 = CIRCLE ( 'NONE', #11220, 0.2000000000000057288 ) ;
#17371 = CARTESIAN_POINT ( 'NONE',  ( 43.81606138205700063, -36.11063010576116739, 71.66210679335823386 ) ) ;
#17372 = ORIENTED_EDGE ( 'NONE', *, *, #21996, .F. ) ;
#17373 = ORIENTED_EDGE ( 'NONE', *, *, #11295, .F. ) ;
#17374 = CARTESIAN_POINT ( 'NONE',  ( 36.11133435605973574, -14.00384086642191583, 70.60699637195608602 ) ) ;
#17375 = DIRECTION ( 'NONE',  ( 0.000000000000000000, 1.000000000000000000, -2.999999999999999839E-15 ) ) ;
#17376 = CARTESIAN_POINT ( 'NONE',  ( 40.14115730948191185, -12.51368208888610489, 71.32335560751960202 ) ) ;
#17377 = SHAPE_REPRESENTATION ( 'MAS-155', ( #1410, #19529, #25260, #9672, #24436, #12540, #14573, #16229, #1822, #8430, #3471, #4313, #10069, #10471 ), #18699 ) ;
#17378 = FILL_AREA_STYLE_COLOUR ( '', #21130 ) ;
#17379 = ORIENTED_EDGE ( 'NONE', *, *, #4182, .F. ) ;
#17380 = DIRECTION ( 'NONE',  ( -7.071067811865477305E-16, 0.4341746501209515774, 0.9008287146801823297 ) ) ;
#17381 = CARTESIAN_POINT ( 'NONE',  ( 31.81606138205700418, 38.19123852234598360, 71.05501292736988717 ) ) ;
#17382 = EDGE_CURVE ( 'NONE', #24915, #1030, #1810, .T. ) ;
#17383 = CARTESIAN_POINT ( 'NONE',  ( 38.26194895904383486, -23.01368208888610312, 69.04448340153878405 ) ) ;
#17384 = ORIENTED_EDGE ( 'NONE', *, *, #111, .F. ) ;
#17385 = VECTOR ( 'NONE', #8368, 1000.000000000000000 ) ;
#17386 = CARTESIAN_POINT ( 'NONE',  ( 31.81606138205700418, 36.92314894770293421, 79.37823623207323465 ) ) ;
#17387 = CARTESIAN_POINT ( 'NONE',  ( 38.37017380507020192, 1.986317911113890444, 73.11602215082119471 ) ) ;
#17388 = DIRECTION ( 'NONE',  ( 0.000000000000000000, 0.7540134720837716742, 0.6568589528324746407 ) ) ;
#17389 = CIRCLE ( 'NONE', #14516, 4.000000000000000000 ) ;
#17390 = DIRECTION ( 'NONE',  ( 1.000000000000000000, 1.000000000000000078E-15, 0.000000000000000000 ) ) ;
#17391 = AXIS2_PLACEMENT_3D ( 'NONE', #19567, #17776, #15189 ) ;
#17392 = AXIS2_PLACEMENT_3D ( 'NONE', #20072, #18027, #8489 ) ;
#17393 = CARTESIAN_POINT ( 'NONE',  ( 37.09309150775561648, -5.616297516291425929, 83.29717550927296088 ) ) ;
#17394 = CARTESIAN_POINT ( 'NONE',  ( 39.31564783533279694, -15.30384086642191477, 70.72433947564853440 ) ) ;
#17395 = CARTESIAN_POINT ( 'NONE',  ( 40.14115730948191185, -0.5136820888861047818, 71.32335560751961623 ) ) ;
#17396 = ORIENTED_EDGE ( 'NONE', *, *, #1387, .T. ) ;
#17397 = CARTESIAN_POINT ( 'NONE',  ( 40.81606138205700773, -31.05876147765399864, 75.30501292737010033 ) ) ;
#17398 = CIRCLE ( 'NONE', #12121, 0.2000000000000057288 ) ;
#17399 = PLANE ( 'NONE',  #20563 ) ;
#17400 = VERTEX_POINT ( 'NONE', #4012 ) ;
#17401 = EDGE_LOOP ( 'NONE', ( #11609, #21648, #22212, #9748 ) ) ;
#17402 = CARTESIAN_POINT ( 'NONE',  ( 40.55423172469004101, -27.20384086642191690, 70.70992431699446001 ) ) ;
#17403 = VECTOR ( 'NONE', #12553, 1000.000000000000000 ) ;
#17404 = CARTESIAN_POINT ( 'NONE',  ( 37.80618814713140097, 0.08631791111389161553, 73.13360434286904876 ) ) ;
#17405 = CARTESIAN_POINT ( 'NONE',  ( 40.52078840805428683, -0.6136820888861042045, 70.60699637195608602 ) ) ;
#17406 = ORIENTED_EDGE ( 'NONE', *, *, #7043, .T. ) ;
#17407 = DIRECTION ( 'NONE',  ( -2.453269466693404537E-16, 0.7071067811865489050, -0.7071067811865460184 ) ) ;
#17408 = CARTESIAN_POINT ( 'NONE',  ( 39.41296390513587511, -3.203840866421912903, 71.08074471024443142 ) ) ;
#17409 = DIRECTION ( 'NONE',  ( -1.786044098272412642E-16, -0.4425581086832399702, 0.8967398287344627850 ) ) ;
#17410 = ORIENTED_EDGE ( 'NONE', *, *, #11243, .F. ) ;
#17411 = VECTOR ( 'NONE', #4346, 1000.000000000000000 ) ;
#17412 = DIRECTION ( 'NONE',  ( 0.000000000000000000, -3.469446951953613400E-15, -1.000000000000000000 ) ) ;
#17413 = MANIFOLD_SOLID_BREP ( 'NONE', #24953 ) ;
#17414 = CARTESIAN_POINT ( 'NONE',  ( 44.06606138205700063, 40.39281886181299797, 83.30501292736984453 ) ) ;
#17415 = EDGE_CURVE ( 'NONE', #15653, #8578, #6573, .T. ) ;
#17416 = CARTESIAN_POINT ( 'NONE',  ( 40.52078840805429394, -13.00384086642191761, 72.15350918040381600 ) ) ;
#17417 = DIRECTION ( 'NONE',  ( 0.000000000000000000, -3.289120579329467819E-15, -1.000000000000000000 ) ) ;
#17418 = CARTESIAN_POINT ( 'NONE',  ( 45.06606138205697931, -5.918777154956152309, -5.916875169744970187 ) ) ;
#17419 = CARTESIAN_POINT ( 'NONE',  ( 39.75915168707250302, -16.71368208888609885, 70.26145752964251301 ) ) ;
#17420 = DIRECTION ( 'NONE',  ( 0.000000000000000000, 0.3299742535180963943, -0.9439899321577402969 ) ) ;
#17421 = CARTESIAN_POINT ( 'NONE',  ( 43.23147868389327897, 41.67000142393845152, 79.87823623207322044 ) ) ;
#17422 = AXIS2_PLACEMENT_3D ( 'NONE', #25000, #23208, #23081 ) ;
#17423 = ORIENTED_EDGE ( 'NONE', *, *, #18913, .T. ) ;
#17424 = DIRECTION ( 'NONE',  ( -1.000000000000000000, -2.999999999999999839E-15, 0.000000000000000000 ) ) ;
#17425 = AXIS2_PLACEMENT_3D ( 'NONE', #3078, #22666, #10823 ) ;
#17426 = CARTESIAN_POINT ( 'NONE',  ( 36.49096545463212493, -4.103840866421911038, 71.32335560751963044 ) ) ;
#17427 = APPLICATION_PROTOCOL_DEFINITION ( 'draft international standard', 'automotive_design', 1998, #16546 ) ;
#17428 = CARTESIAN_POINT ( 'NONE',  ( 33.10058206061923869, 3.250575416431807696, 6.144373406101647284 ) ) ;
#17429 = EDGE_CURVE ( 'NONE', #5934, #8968, #8018, .T. ) ;
#17430 = CARTESIAN_POINT ( 'NONE',  ( 37.25202387243752611, -21.21368208888610241, 70.00779233799262613 ) ) ;
#17431 = DIRECTION ( 'NONE',  ( 0.000000000000000000, 1.000000000000000000, 0.000000000000000000 ) ) ;
#17432 = CIRCLE ( 'NONE', #23994, 0.7500000000000041078 ) ;
#17433 = ADVANCED_FACE ( 'NONE', ( #10575 ), #254, .F. ) ;
#17434 = ADVANCED_FACE ( 'NONE', ( #24082 ), #23831, .F. ) ;
#17435 = CARTESIAN_POINT ( 'NONE',  ( 36.49096545463212493, -16.10384086642191548, 71.32335560751961623 ) ) ;
#17436 = ADVANCED_FACE ( 'NONE', ( #18056 ), #10077, .T. ) ;
#17437 = CARTESIAN_POINT ( 'NONE',  ( 38.31606138205700063, -5.204193249396277032, 83.31006292736994112 ) ) ;
#17438 = STYLED_ITEM ( 'NONE', ( #14034 ), #6771 ) ;
#17439 = CARTESIAN_POINT ( 'NONE',  ( 37.25202387243752611, -15.21368208888610063, 70.00779233799262613 ) ) ;
#17440 = VERTEX_POINT ( 'NONE', #22159 ) ;
#17441 = CARTESIAN_POINT ( 'NONE',  ( 40.33642880535524000, -24.31368208888611093, 72.77780686321125359 ) ) ;
#17442 = ORIENTED_EDGE ( 'NONE', *, *, #5948, .F. ) ;
#17443 = FACE_OUTER_BOUND ( 'NONE', #13417, .T. ) ;
#17444 = VECTOR ( 'NONE', #2577, 1000.000000000000000 ) ;
#17445 = DIRECTION ( 'NONE',  ( 1.218693434051482139E-16, -0.4425581086832393041, 0.8967398287344630070 ) ) ;
#17446 = CARTESIAN_POINT ( 'NONE',  ( 37.38336156205273397, -25.90384086642191264, 70.63227792289245599 ) ) ;
#17447 = ORIENTED_EDGE ( 'NONE', *, *, #8938, .F. ) ;
#17448 = ORIENTED_EDGE ( 'NONE', *, *, #21979, .T. ) ;
#17449 = DIRECTION ( 'NONE',  ( 0.000000000000000000, 0.000000000000000000, -1.000000000000000000 ) ) ;
#17450 = COLOUR_RGB ( '', 0.40784314, 0.44705882, 0.49803922) ;
#17451 = CARTESIAN_POINT ( 'NONE',  ( 32.56606138205700773, 42.82479937715250173, 82.59790614618330551 ) ) ;
#17452 = EDGE_LOOP ( 'NONE', ( #13798, #3622, #21562, #7451 ) ) ;
#17453 = EDGE_CURVE ( 'NONE', #9754, #18371, #11884, .T. ) ;
#17454 = LINE ( 'NONE', #19242, #10236 ) ;
#17455 = CARTESIAN_POINT ( 'NONE',  ( 36.87297107704149823, 0.09615913357809147133, 70.26145752964255564 ) ) ;
#17456 = CARTESIAN_POINT ( 'NONE',  ( 45.81606138205700063, -26.74044063519535186, 82.55501292737007191 ) ) ;
#17457 = CYLINDRICAL_SURFACE ( 'NONE', #13103, 1.249999999999998890 ) ;
#17458 = B_SPLINE_CURVE_WITH_KNOTS ( 'NONE', 3,
 ( #2953, #10715, #10838, #1286, #18561, #4652, #1024, #8908, #18435, #766, #4772, #24717, #16748, #24583, #20755, #22675 ),
 .UNSPECIFIED., .F., .F.,
 ( 4, 2, 2, 2, 2, 2, 2, 4 ),
 ( 0.000000000000000000, 0.1250000000000006106, 0.2499999999999996947, 0.3750000000000002776, 0.5000000000000008882, 0.6249999999999982236, 0.7499999999999987788, 1.000000000000000000 ),
 .UNSPECIFIED. ) ;
#17459 = ORIENTED_EDGE ( 'NONE', *, *, #7450, .T. ) ;
#17460 = EDGE_LOOP ( 'NONE', ( #8186, #7057, #20350, #19542 ) ) ;
#17461 = LINE ( 'NONE', #9358, #11265 ) ;
#17462 = MECHANICAL_DESIGN_GEOMETRIC_PRESENTATION_REPRESENTATION (  '', ( #19923 ), #24023 ) ;
#17463 = DIRECTION ( 'NONE',  ( 1.000000000000000000, -0.000000000000000000, 0.000000000000000000 ) ) ;
#17464 = CARTESIAN_POINT ( 'NONE',  ( 43.81606138205700063, 44.92314894770293421, 79.37823623207320622 ) ) ;
#17465 = VECTOR ( 'NONE', #8957, 1000.000000000000000 ) ;
#17466 = AXIS2_PLACEMENT_3D ( 'NONE', #16797, #1333, #20801 ) ;
#17467 = DIRECTION ( 'NONE',  ( -1.000000000000000000, -1.000000000000000078E-15, 0.000000000000000000 ) ) ;
#17468 = ORIENTED_EDGE ( 'NONE', *, *, #13965, .T. ) ;
#17469 = DIRECTION ( 'NONE',  ( 2.776799322558808202E-15, -0.8967398287344627850, -0.4425581086832400257 ) ) ;
#17470 = CIRCLE ( 'NONE', #4725, 1.000000000000000888 ) ;
#17471 = DIRECTION ( 'NONE',  ( 1.327674326049719602E-15, -0.4425581086832399147, 0.8967398287344627850 ) ) ;
#17472 = PLANE ( 'NONE',  #4803 ) ;
#17473 = ADVANCED_FACE ( 'NONE', ( #21911 ), #12525, .T. ) ;
#17474 = CARTESIAN_POINT ( 'NONE',  ( 38.93987200065210175, -6.803840866421912104, 72.33091598616827866 ) ) ;
#17475 = ADVANCED_FACE ( 'NONE', ( #10195 ), #8395, .T. ) ;
#17476 = ORIENTED_EDGE ( 'NONE', *, *, #20550, .F. ) ;
#17477 = DIRECTION ( 'NONE',  ( -2.122643018205887308E-17, 1.000000000000000000, -3.120611096041553009E-15 ) ) ;
#17478 = VERTEX_POINT ( 'NONE', #2694 ) ;
#17479 = ORIENTED_EDGE ( 'NONE', *, *, #14555, .F. ) ;
#17480 = CARTESIAN_POINT ( 'NONE',  ( 41.31606138205700063, 7.535758204303438568, 66.26723409915207696 ) ) ;
#17481 = CARTESIAN_POINT ( 'NONE',  ( 37.89291511884476904, -13.11368208888610454, 70.26206559358661252 ) ) ;
#17482 =( GEOMETRIC_REPRESENTATION_CONTEXT ( 3 ) GLOBAL_UNCERTAINTY_ASSIGNED_CONTEXT ( ( #5148 ) ) GLOBAL_UNIT_ASSIGNED_CONTEXT ( ( #8304, #19765, #8053 ) ) REPRESENTATION_CONTEXT ( 'NONE', 'WORKASPACE' ) );
#17483 = CARTESIAN_POINT ( 'NONE',  ( 37.25260217561390874, -13.61368208888610098, 71.78268878715392987 ) ) ;
#17484 = ORIENTED_EDGE ( 'NONE', *, *, #24182, .T. ) ;
#17485 = ORIENTED_EDGE ( 'NONE', *, *, #22313, .F. ) ;
#17486 = CARTESIAN_POINT ( 'NONE',  ( 43.81606138205700063, 34.92314894770293421, 80.37823623207323465 ) ) ;
#17487 = DIRECTION ( 'NONE',  ( 0.000000000000000000, 2.999999999999999839E-15, 1.000000000000000000 ) ) ;
#17488 = ORIENTED_EDGE ( 'NONE', *, *, #25452, .T. ) ;
#17489 = EDGE_CURVE ( 'NONE', #21396, #24541, #5414, .T. ) ;
#17490 = CARTESIAN_POINT ( 'NONE',  ( 42.96606138205697789, -5.898435835062210586, -2.003809078978638247 ) ) ;
#17491 = CARTESIAN_POINT ( 'NONE',  ( 38.37017380507018771, -17.60384086642190837, 69.64448340153877837 ) ) ;
#17492 = VECTOR ( 'NONE', #660, 1000.000000000000000 ) ;
#17493 = DIRECTION ( 'NONE',  ( 0.000000000000000000, -0.6568589528324746407, 0.7540134720837717852 ) ) ;
#17494 = CARTESIAN_POINT ( 'NONE',  ( 37.69225076346193504, -17.81368208888610383, 72.33091598616826445 ) ) ;
#17495 = ORIENTED_EDGE ( 'NONE', *, *, #17637, .T. ) ;
#17496 = LINE ( 'NONE', #3560, #15749 ) ;
#17497 = CARTESIAN_POINT ( 'NONE',  ( 37.25202387243752611, -11.21368208888610241, 70.00779233799262613 ) ) ;
#17498 = ADVANCED_FACE ( 'NONE', ( #16104 ), #22714, .T. ) ;
#17499 = CARTESIAN_POINT ( 'NONE',  ( 32.81606138205700773, -32.95845724189726411, 59.23979596822106686 ) ) ;
#17500 = LINE ( 'NONE', #9519, #13271 ) ;
#17501 = CARTESIAN_POINT ( 'NONE',  ( 38.57734783014581836, -5.216343248895277895, 82.80503566129729620 ) ) ;
#17502 = FACE_OUTER_BOUND ( 'NONE', #23990, .T. ) ;
#17503 = AXIS2_PLACEMENT_3D ( 'NONE', #16233, #6449, #18427 ) ;
#17504 = AXIS2_PLACEMENT_3D ( 'NONE', #5689, #9822, #24202 ) ;
#17505 = DIRECTION ( 'NONE',  ( 1.000000000000000000, -6.018531076210090146E-31, -1.734723475976804876E-16 ) ) ;
#17506 = ORIENTED_EDGE ( 'NONE', *, *, #5240, .F. ) ;
#17507 = LINE ( 'NONE', #9903, #21006 ) ;
#17508 = ORIENTED_EDGE ( 'NONE', *, *, #24798, .T. ) ;
#17509 = VERTEX_POINT ( 'NONE', #22285 ) ;
#17510 = CARTESIAN_POINT ( 'NONE',  ( 40.52078840805429394, -13.00384086642191761, 72.15350918040381600 ) ) ;
#17511 = ORIENTED_EDGE ( 'NONE', *, *, #12866, .F. ) ;
#17512 = CARTESIAN_POINT ( 'NONE',  ( 43.31606138205700063, -36.11063010576116739, 71.66210679335823386 ) ) ;
#17513 = CARTESIAN_POINT ( 'NONE',  ( 36.87297107704152666, -15.71368208888610596, 72.49904802271740323 ) ) ;
#17514 = ORIENTED_EDGE ( 'NONE', *, *, #25340, .T. ) ;
#17515 = DIRECTION ( 'NONE',  ( -1.156482317317870492E-16, -0.4425581086832399702, 0.8967398287344626739 ) ) ;
#17516 = LINE ( 'NONE', #25341, #20336 ) ;
#17517 = CARTESIAN_POINT ( 'NONE',  ( 36.29569395875879678, -21.31368208888610027, 69.98269868914867686 ) ) ;
#17518 = EDGE_CURVE ( 'NONE', #22231, #20891, #18431, .T. ) ;
#17519 = DIRECTION ( 'NONE',  ( -1.000000000000000000, -1.000000000000000078E-15, 0.000000000000000000 ) ) ;
#17520 = EDGE_CURVE ( 'NONE', #2724, #4754, #18313, .T. ) ;
#17521 = DIRECTION ( 'NONE',  ( 2.602085213965210642E-15, -0.8967398287344635621, -0.4425581086832386379 ) ) ;
#17522 = CARTESIAN_POINT ( 'NONE',  ( 40.81606138205700773, -31.05876147765399864, 75.30501292737010033 ) ) ;
#17523 = EDGE_CURVE ( 'NONE', #18244, #16267, #634, .T. ) ;
#17524 = CARTESIAN_POINT ( 'NONE',  ( 32.31606138205700063, 10.06218483883314718, 67.80501292737497465 ) ) ;
#17525 =( NAMED_UNIT ( * ) SI_UNIT ( $, .STERADIAN. ) SOLID_ANGLE_UNIT ( ) );
#17526 = CARTESIAN_POINT ( 'NONE',  ( 33.31606138205700773, -1.357181138186128067, 82.80501292736991559 ) ) ;
#17527 = FACE_OUTER_BOUND ( 'NONE', #19189, .T. ) ;
#17528 = CARTESIAN_POINT ( 'NONE',  ( 37.25260217561390874, -12.00384086642191228, 70.97781676520601479 ) ) ;
#17529 = CARTESIAN_POINT ( 'NONE',  ( 39.75915168707250302, 1.286317911113898260, 70.26145752964255564 ) ) ;
#17530 = ORIENTED_EDGE ( 'NONE', *, *, #10395, .T. ) ;
#17531 = CARTESIAN_POINT ( 'NONE',  ( 40.31606138205700773, -31.05876147765400574, 73.55501292737010033 ) ) ;
#17532 = ADVANCED_FACE ( 'NONE', ( #12261, #2444 ), #10320, .F. ) ;
#17533 = LINE ( 'NONE', #5932, #387 ) ;
#17534 = ORIENTED_EDGE ( 'NONE', *, *, #23422, .T. ) ;
#17535 = EDGE_LOOP ( 'NONE', ( #6896, #11313, #4218, #10942 ) ) ;
#17536 = CARTESIAN_POINT ( 'NONE',  ( 39.98359781491296161, 0.7961591335780872081, 70.89533451361948835 ) ) ;
#17537 = CARTESIAN_POINT ( 'NONE',  ( 39.41296390513587511, -26.41368208888610170, 71.67976084211548482 ) ) ;
#17538 = PRODUCT_DEFINITION_SHAPE ( 'NONE', 'NONE',  #3162 ) ;
#17539 = CARTESIAN_POINT ( 'NONE',  ( 36.29569395875879678, -5.313682088886097610, 69.98269868914869107 ) ) ;
#17540 = VERTEX_POINT ( 'NONE', #2948 ) ;
#17541 = LINE ( 'NONE', #15590, #23458 ) ;
#17542 = CARTESIAN_POINT ( 'NONE',  ( 39.31564783533279694, -5.303840866421911215, 70.72433947564853440 ) ) ;
#17543 = DIRECTION ( 'NONE',  ( 1.000000000000000000, 0.000000000000000000, 0.000000000000000000 ) ) ;
#17544 = ORIENTED_EDGE ( 'NONE', *, *, #2860, .T. ) ;
#17545 = CARTESIAN_POINT ( 'NONE',  ( 36.31606138205700063, -30.30876147765399864, 75.30501292736995822 ) ) ;
#17546 = LINE ( 'NONE', #17414, #5916 ) ;
#17547 = CARTESIAN_POINT ( 'NONE',  ( 39.73277004305197124, -11.40384086642191086, 69.52238214136768590 ) ) ;
#17548 = DIRECTION ( 'NONE',  ( -1.000000000000000000, -3.091505625455828697E-15, -4.515976121274772923E-17 ) ) ;
#17549 =( NAMED_UNIT ( * ) PLANE_ANGLE_UNIT ( ) SI_UNIT ( $, .RADIAN. ) );
#17550 = CARTESIAN_POINT ( 'NONE',  ( 38.82593461698262871, -10.91368208888609992, 69.62690120949091011 ) ) ;
#17551 = LINE ( 'NONE', #1554, #18803 ) ;
#17552 = DIRECTION ( 'NONE',  ( 0.000000000000000000, 1.000000000000000000, 0.000000000000000000 ) ) ;
#17553 = CARTESIAN_POINT ( 'NONE',  ( 44.81606138205700063, 41.44123852234599070, 73.55501292736987295 ) ) ;
#17554 = CARTESIAN_POINT ( 'NONE',  ( 38.82593461698264292, -2.703840866421916012, 73.13360434286904876 ) ) ;
#17555 = APPLICATION_PROTOCOL_DEFINITION ( 'draft international standard', 'automotive_design', 1998, #20659 ) ;
#17556 = LINE ( 'NONE', #3509, #24386 ) ;
#17557 = CARTESIAN_POINT ( 'NONE',  ( 37.80618814713140097, -17.91368208888609814, 73.13360434286903455 ) ) ;
#17558 = DIRECTION ( 'NONE',  ( 0.000000000000000000, -2.999999999999999839E-15, -1.000000000000000000 ) ) ;
#17559 = EDGE_CURVE ( 'NONE', #3043, #6859, #20485, .T. ) ;
#17560 = CARTESIAN_POINT ( 'NONE',  ( 39.29254315202757653, -18.80384086642191477, 72.81632618279321889 ) ) ;
#17561 = CARTESIAN_POINT ( 'NONE',  ( 36.99159426505191561, -5.700015143112625360, 83.29877568887539496 ) ) ;
#17562 = CARTESIAN_POINT ( 'NONE',  ( 38.37017380507020192, -20.01368208888610667, 73.11602215082116629 ) ) ;
#17563 = ORIENTED_EDGE ( 'NONE', *, *, #7692, .F. ) ;
#17564 = CARTESIAN_POINT ( 'NONE',  ( 36.36258059203031934, -19.71368208888610951, 72.86986841596736042 ) ) ;
#17565 = VERTEX_POINT ( 'NONE', #18806 ) ;
#17566 = DIRECTION ( 'NONE',  ( -9.999999999999998805E-16, 0.9439899321577399638, 0.3299742535180969494 ) ) ;
#17567 = CARTESIAN_POINT ( 'NONE',  ( 44.06606138205700063, -26.74044063519535186, 84.30501292737007191 ) ) ;
#17568 = CARTESIAN_POINT ( 'NONE',  ( 38.37017380507018771, -27.60384086642191548, 70.24448340153875847 ) ) ;
#17569 = ORIENTED_EDGE ( 'NONE', *, *, #12737, .T. ) ;
#17570 = ORIENTED_EDGE ( 'NONE', *, *, #24517, .T. ) ;
#17571 = CARTESIAN_POINT ( 'NONE',  ( 37.31606138205698642, -10.17000407126884376, 36.59108960988216808 ) ) ;
#17572 = CARTESIAN_POINT ( 'NONE',  ( 35.64099152588522657, -8.607181138186998481, 83.30501292737001506 ) ) ;
#17573 = EDGE_LOOP ( 'NONE', ( #17641, #17870, #2023, #12733 ) ) ;
#17574 = FILL_AREA_STYLE_COLOUR ( '', #3230 ) ;
#17575 = CARTESIAN_POINT ( 'NONE',  ( 36.98690846071097127, -27.80384086642191477, 69.45876917294174291 ) ) ;
#17576 = EDGE_CURVE ( 'NONE', #13623, #9234, #18683, .T. ) ;
#17577 =( NAMED_UNIT ( * ) SI_UNIT ( $, .STERADIAN. ) SOLID_ANGLE_UNIT ( ) );
#17578 = CARTESIAN_POINT ( 'NONE',  ( 40.52078840805428683, -0.6136820888861042045, 70.60699637195608602 ) ) ;
#17579 = DIRECTION ( 'NONE',  ( 0.000000000000000000, -0.7540134720837725624, -0.6568589528324736415 ) ) ;
#17580 = ORIENTED_EDGE ( 'NONE', *, *, #20191, .T. ) ;
#17581 = EDGE_CURVE ( 'NONE', #14979, #6943, #5861, .T. ) ;
#17582 = VERTEX_POINT ( 'NONE', #20746 ) ;
#17583 = AXIS2_PLACEMENT_3D ( 'NONE', #23749, #23993, #16140 ) ;
#17584 = AXIS2_PLACEMENT_3D ( 'NONE', #11775, #525, #21928 ) ;
#17585 = DIRECTION ( 'NONE',  ( 0.000000000000000000, 1.000000000000000000, -3.469446951953701358E-15 ) ) ;
#17586 = LINE ( 'NONE', #23362, #23722 ) ;
#17587 = CARTESIAN_POINT ( 'NONE',  ( 39.75915168707251723, -20.90384086642190908, 72.49904802271738902 ) ) ;
#17588 = CARTESIAN_POINT ( 'NONE',  ( 44.81606138205700063, -34.55876147765400930, 73.55501292737011454 ) ) ;
#17589 = ORIENTED_EDGE ( 'NONE', *, *, #24661, .F. ) ;
#17590 = CARTESIAN_POINT ( 'NONE',  ( 44.81606138205700063, -34.55876147765400930, 73.55501292737011454 ) ) ;
#17591 = EDGE_CURVE ( 'NONE', #170, #1658, #12773, .T. ) ;
#17592 = DIRECTION ( 'NONE',  ( -0.1733269559585470521, -3.077057697073492856E-15, -0.9848643390529193686 ) ) ;
#17593 = CARTESIAN_POINT ( 'NONE',  ( 40.81606138205700773, 37.44123852234599781, 74.30501292736988717 ) ) ;
#17594 = CARTESIAN_POINT ( 'NONE',  ( 38.00113996487112189, -7.703840866421914235, 70.22690120949091863 ) ) ;
#17595 = ORIENTED_EDGE ( 'NONE', *, *, #1368, .T. ) ;
#17596 = DIRECTION ( 'NONE',  ( 0.000000000000000000, -2.999999999999999839E-15, -1.000000000000000000 ) ) ;
#17597 = VERTEX_POINT ( 'NONE', #8777 ) ;
#17598 = ORIENTED_EDGE ( 'NONE', *, *, #523, .T. ) ;
#17599 = LINE ( 'NONE', #7811, #20887 ) ;
#17600 = CARTESIAN_POINT ( 'NONE',  ( 39.31564783533280405, -14.31368208888609850, 72.03616607671141026 ) ) ;
#17601 = AXIS2_PLACEMENT_3D ( 'NONE', #18589, #10872, #15101 ) ;
#17602 = VECTOR ( 'NONE', #10682, 1000.000000000000000 ) ;
#17603 = CARTESIAN_POINT ( 'NONE',  ( 38.37017380507020192, -8.013682088886101340, 72.51602215082118619 ) ) ;
#17604 = EDGE_LOOP ( 'NONE', ( #13449, #11290, #23185, #17981 ) ) ;
#17605 = ORIENTED_EDGE ( 'NONE', *, *, #11381, .T. ) ;
#17606 = DIRECTION ( 'NONE',  ( 1.849283715844614702E-16, -0.8212051873014210024, -0.5706330172266920187 ) ) ;
#17607 = CARTESIAN_POINT ( 'NONE',  ( 43.31606138205700063, -26.06829118875199569, 75.80501292736998664 ) ) ;
#17608 = VERTEX_POINT ( 'NONE', #11086 ) ;
#17609 = CARTESIAN_POINT ( 'NONE',  ( 39.75915168707250302, 1.286317911113898260, 70.26145752964255564 ) ) ;
#17610 = CARTESIAN_POINT ( 'NONE',  ( 37.69796330110505522, -16.50384086642191761, 73.09843995877329803 ) ) ;
#17611 = EDGE_CURVE ( 'NONE', #19039, #10246, #1716, .T. ) ;
#17612 = EDGE_CURVE ( 'NONE', #2946, #15409, #3788, .T. ) ;
#17613 = CARTESIAN_POINT ( 'NONE',  ( 29.81606138205696865, -3.028410647649181442, 0.3252050635115383281 ) ) ;
#17614 = CARTESIAN_POINT ( 'NONE',  ( 39.24876120206128860, -16.71368208888610241, 70.63227792289245599 ) ) ;
#17615 = EDGE_CURVE ( 'NONE', #2345, #3400, #15733, .T. ) ;
#17616 = EDGE_CURVE ( 'NONE', #10282, #11605, #24843, .T. ) ;
#17617 = ADVANCED_FACE ( 'NONE', ( #1281 ), #24328, .T. ) ;
#17618 = ORIENTED_EDGE ( 'NONE', *, *, #3730, .T. ) ;
#17619 = CARTESIAN_POINT ( 'NONE',  ( 45.06606138205707879, -38.42645682328033985, 63.90656833300437256 ) ) ;
#17620 = CARTESIAN_POINT ( 'NONE',  ( 37.69796330110504101, -17.11368208888610098, 69.66206559358663242 ) ) ;
#17621 = DIRECTION ( 'NONE',  ( 3.491481338843135327E-15, 1.000000000000000000, -2.999999999999999839E-15 ) ) ;
#17622 = AXIS2_PLACEMENT_3D ( 'NONE', #6068, #21651, #15729 ) ;
#17623 = DIRECTION ( 'NONE',  ( -1.000000000000000000, 0.000000000000000000, 0.000000000000000000 ) ) ;
#17624 = AXIS2_PLACEMENT_3D ( 'NONE', #24364, #24484, #1179 ) ;
#17625 = CIRCLE ( 'NONE', #21309, 1.000000000000011990 ) ;
#17626 = FACE_OUTER_BOUND ( 'NONE', #17727, .T. ) ;
#17627 = CARTESIAN_POINT ( 'NONE',  ( 43.81608638205700146, -2.373793412309109563, 19.60611914621674146 ) ) ;
#17628 = ADVANCED_FACE ( 'NONE', ( #10710 ), #21488, .T. ) ;
#17629 = ADVANCED_FACE ( 'NONE', ( #22670 ), #883, .T. ) ;
#17630 = DIRECTION ( 'NONE',  ( 0.000000000000000000, 0.6568589528324747517, -0.7540134720837718962 ) ) ;
#17631 = EDGE_LOOP ( 'NONE', ( #7739, #6476, #15627, #445 ) ) ;
#17632 = DIRECTION ( 'NONE',  ( 1.000000000000000000, 0.000000000000000000, 0.000000000000000000 ) ) ;
#17633 = ORIENTED_EDGE ( 'NONE', *, *, #12044, .T. ) ;
#17634 = ORIENTED_EDGE ( 'NONE', *, *, #11646, .F. ) ;
#17635 = CARTESIAN_POINT ( 'NONE',  ( 39.02088643472237806, -8.703840866421918676, 73.73360434286902887 ) ) ;
#17636 = VERTEX_POINT ( 'NONE', #17009 ) ;
#17637 = EDGE_CURVE ( 'NONE', #18276, #6436, #16480, .T. ) ;
#17638 = LINE ( 'NONE', #17899, #1710 ) ;
#17639 = CARTESIAN_POINT ( 'NONE',  ( 36.49096545463212493, -15.51368208888610667, 71.43714994484034264 ) ) ;
#17640 = VECTOR ( 'NONE', #17886, 1000.000000000000000 ) ;
#17641 = ORIENTED_EDGE ( 'NONE', *, *, #13741, .T. ) ;
#17642 = DIRECTION ( 'NONE',  ( -1.000000000000000000, -2.999999999999999839E-15, 0.000000000000000000 ) ) ;
#17643 = CARTESIAN_POINT ( 'NONE',  ( 42.81606138205700063, 16.19123852234699967, 69.30501292736995822 ) ) ;
#17644 = CARTESIAN_POINT ( 'NONE',  ( 36.98690846071097837, -23.81368208888611093, 73.30173637941817333 ) ) ;
#17645 = ORIENTED_EDGE ( 'NONE', *, *, #9738, .F. ) ;
#17646 = VECTOR ( 'NONE', #24171, 1000.000000000000000 ) ;
#17647 =( NAMED_UNIT ( * ) PLANE_ANGLE_UNIT ( ) SI_UNIT ( $, .RADIAN. ) );
#17648 = CARTESIAN_POINT ( 'NONE',  ( 35.31606138205700773, 3.536347952325769040, 64.10938348997790115 ) ) ;
#17649 = CARTESIAN_POINT ( 'NONE',  ( 31.81606138205700418, -38.55876147765400930, 73.30501292737012875 ) ) ;
#17650 = DIRECTION ( 'NONE',  ( 2.312964634635740294E-15, 2.999999999999999839E-15, 1.000000000000000000 ) ) ;
#17651 = DIRECTION ( 'NONE',  ( 1.000000000000000000, 1.734723475976804876E-16, -1.734723475976814737E-16 ) ) ;
#17652 = CARTESIAN_POINT ( 'NONE',  ( 37.31647492878124694, -12.30384086642191299, 72.03616607671141026 ) ) ;
#17653 = CARTESIAN_POINT ( 'NONE',  ( 39.98359781491296161, -2.413682088886103472, 71.86517103874048473 ) ) ;
#17654 = VECTOR ( 'NONE', #14987, 1000.000000000000227 ) ;
#17655 = VERTEX_POINT ( 'NONE', #14559 ) ;
#17656 = CARTESIAN_POINT ( 'NONE',  ( 38.44690133353662276, -22.22127907754186893, 75.81001292736998209 ) ) ;
#17657 = DIRECTION ( 'NONE',  ( 0.000000000000000000, 0.5706330172266919076, -0.8212051873014208914 ) ) ;
#17658 = VERTEX_POINT ( 'NONE', #22417 ) ;
#17659 = VERTEX_POINT ( 'NONE', #12644 ) ;
#17660 = ADVANCED_FACE ( 'NONE', ( #14677 ), #22545, .F. ) ;
#17661 = CARTESIAN_POINT ( 'NONE',  ( 39.29254315202757653, -0.8038408664219134359, 72.81632618279323310 ) ) ;
#17662 = VECTOR ( 'NONE', #23910, 1000.000000000000000 ) ;
#17663 = PRODUCT_DEFINITION ( 'UNKNOWN', '', #6371, #14393 ) ;
#17664 = CARTESIAN_POINT ( 'NONE',  ( 37.69225076346193504, -21.81368208888610027, 72.33091598616826445 ) ) ;
#17665 = CARTESIAN_POINT ( 'NONE',  ( 36.11133435605973574, -1.613682088886104982, 72.15350918040385864 ) ) ;
#17666 = VERTEX_POINT ( 'NONE', #4229 ) ;
#17667 = DIRECTION ( 'NONE',  ( -1.000000000000000000, 5.204170427930415223E-30, 1.734723475976805122E-15 ) ) ;
#17668 = CARTESIAN_POINT ( 'NONE',  ( 39.38009889167648936, -29.40384086642190908, 70.00779233799262613 ) ) ;
#17669 = PLANE ( 'NONE',  #10588 ) ;
#17670 = ORIENTED_EDGE ( 'NONE', *, *, #20567, .T. ) ;
#17671 = CARTESIAN_POINT ( 'NONE',  ( 32.81606138205700773, 2.191238522347013440, 73.80501292737000085 ) ) ;
#17672 = CARTESIAN_POINT ( 'NONE',  ( 41.31606138205700063, 8.104266321858618838, 55.82104096753806033 ) ) ;
#17673 = CARTESIAN_POINT ( 'NONE',  ( 39.64521430340305841, -8.803840866421916544, 73.30173637941818754 ) ) ;
#17674 = DIRECTION ( 'NONE',  ( 0.000000000000000000, 0.6568589528324747517, -0.7540134720837718962 ) ) ;
#17675 = CIRCLE ( 'NONE', #12336, 2.000000000000001776 ) ;
#17676 = CARTESIAN_POINT ( 'NONE',  ( 36.64852494920107517, -15.41368208888610525, 70.89533451361947414 ) ) ;
#17677 = DIRECTION ( 'NONE',  ( 0.000000000000000000, -2.999999999999999839E-15, -1.000000000000000000 ) ) ;
#17678 = DIRECTION ( 'NONE',  ( 0.000000000000000000, -0.7071067811865489050, 0.7071067811865460184 ) ) ;
#17679 = VECTOR ( 'NONE', #14772, 1000.000000000000000 ) ;
#17680 = FACE_OUTER_BOUND ( 'NONE', #18492, .T. ) ;
#17681 = CARTESIAN_POINT ( 'NONE',  ( 39.98359781491296161, -1.203840866421911127, 70.89533451361947414 ) ) ;
#17682 = CYLINDRICAL_SURFACE ( 'NONE', #6706, 1.250000000000000888 ) ;
#17683 = VECTOR ( 'NONE', #15683, 1000.000000000000000 ) ;
#17684 = CARTESIAN_POINT ( 'NONE',  ( 36.87297107704152666, -21.71368208888610951, 72.49904802271740323 ) ) ;
#17685 = DIRECTION ( 'NONE',  ( 2.442401846778130416E-15, -0.8967398287344627850, -0.4425581086832399147 ) ) ;
#17686 = EDGE_CURVE ( 'NONE', #4783, #7140, #13676, .T. ) ;
#17687 = CARTESIAN_POINT ( 'NONE',  ( 38.82593461698265003, -20.70384086642191335, 73.13360434286903455 ) ) ;
#17688 = FACE_OUTER_BOUND ( 'NONE', #2059, .T. ) ;
#17689 = AXIS2_PLACEMENT_3D ( 'NONE', #1265, #20984, #1127 ) ;
#17690 = ADVANCED_FACE ( 'NONE', ( #22002 ), #8353, .F. ) ;
#17691 = CARTESIAN_POINT ( 'NONE',  ( 37.80618814713140097, -13.91368208888610347, 73.13360434286903455 ) ) ;
#17692 = ORIENTED_EDGE ( 'NONE', *, *, #1676, .T. ) ;
#17693 = CARTESIAN_POINT ( 'NONE',  ( 40.26954217208371034, -20.71368208888610596, 69.89063713639258424 ) ) ;
#17694 = ORIENTED_EDGE ( 'NONE', *, *, #10049, .T. ) ;
#17695 = CARTESIAN_POINT ( 'NONE',  ( 38.38987944808049235, -39.60718113818700203, 83.30501292737011454 ) ) ;
#17696 = CARTESIAN_POINT ( 'NONE',  ( 31.81606138205700418, -36.05876147765410877, 70.30501292737000085 ) ) ;
#17697 = CARTESIAN_POINT ( 'NONE',  ( 39.37952058850012804, -25.00384086642191406, 71.78268878715390144 ) ) ;
#17698 = AXIS2_PLACEMENT_3D ( 'NONE', #257, #8136, #22804 ) ;
#17699 = VERTEX_POINT ( 'NONE', #20067 ) ;
#17700 = VERTEX_POINT ( 'NONE', #8602 ) ;
#17701 = CARTESIAN_POINT ( 'NONE',  ( 38.31606138205700063, 38.69123852234599070, 72.30501292737018559 ) ) ;
#17702 = CARTESIAN_POINT ( 'NONE',  ( 33.66606138205698073, -6.230354416574667376, -1.331254207427787328 ) ) ;
#17703 = ORIENTED_EDGE ( 'NONE', *, *, #19083, .F. ) ;
#17704 = CARTESIAN_POINT ( 'NONE',  ( 46.81606138205697931, -6.570990706613046406, -2.335727660491067503 ) ) ;
#17705 = CARTESIAN_POINT ( 'NONE',  ( 40.33642880535521869, -27.30384086642191477, 69.98269868914864844 ) ) ;
#17706 = VECTOR ( 'NONE', #2735, 1000.000000000000000 ) ;
#17707 = DIRECTION ( 'NONE',  ( 0.000000000000000000, -0.7516416929448823669, -0.6595716529892345914 ) ) ;
#17708 = CARTESIAN_POINT ( 'NONE',  ( 40.33642880535524000, -0.3136820888861093781, 72.77780686321128201 ) ) ;
#17709 = EDGE_CURVE ( 'NONE', #24693, #8218, #14269, .T. ) ;
#17710 = AXIS2_PLACEMENT_3D ( 'NONE', #12390, #12772, #11085 ) ;
#17711 = DIRECTION ( 'NONE',  ( 1.000000000000000000, 0.000000000000000000, 0.000000000000000000 ) ) ;
#17712 = ORIENTED_EDGE ( 'NONE', *, *, #9813, .T. ) ;
#17713 = ORIENTED_EDGE ( 'NONE', *, *, #10716, .F. ) ;
#17714 = CARTESIAN_POINT ( 'NONE',  ( 33.35568666798391746, 2.997371002701979759, 6.110935844446934162 ) ) ;
#17715 = DIRECTION ( 'NONE',  ( -1.000000000000000000, 1.927470528863119788E-16, -5.782411586589358909E-31 ) ) ;
#17716 = CARTESIAN_POINT ( 'NONE',  ( 39.98359781491296161, -21.20384086642190979, 70.89533451361945993 ) ) ;
#17717 = DIRECTION ( 'NONE',  ( 0.000000000000000000, -4.343580702399009298E-14, -1.000000000000000000 ) ) ;
#17718 = EDGE_LOOP ( 'NONE', ( #9762, #24187 ) ) ;
#17719 = DIRECTION ( 'NONE',  ( -1.000000000000000000, -1.734723475976804876E-16, 1.734723475976814737E-16 ) ) ;
#17720 = VECTOR ( 'NONE', #12127, 1000.000000000000000 ) ;
#17721 = CARTESIAN_POINT ( 'NONE',  ( 38.31606138205700773, -21.82678658219787948, 29.70634659473178019 ) ) ;
#17722 = VERTEX_POINT ( 'NONE', #2775 ) ;
#17723 = CARTESIAN_POINT ( 'NONE',  ( 39.41296390513587511, -3.203840866421912903, 71.08074471024443142 ) ) ;
#17724 = CARTESIAN_POINT ( 'NONE',  ( 43.81606138205700063, 35.44123852234597649, 67.80501292736990138 ) ) ;
#17725 = ORIENTED_EDGE ( 'NONE', *, *, #8620, .F. ) ;
#17726 = DIRECTION ( 'NONE',  ( 0.000000000000000000, -0.8967398287344631180, -0.4425581086832393041 ) ) ;
#17727 = EDGE_LOOP ( 'NONE', ( #19576, #15113, #21213, #5475, #869 ) ) ;
#17728 = VERTEX_POINT ( 'NONE', #12101 ) ;
#17729 = CARTESIAN_POINT ( 'NONE',  ( 38.09940268710882094, 37.69123852234599781, 70.07393250355386272 ) ) ;
#17730 = CARTESIAN_POINT ( 'NONE',  ( 39.37952058850012804, -14.61368208888610098, 70.97781676520601479 ) ) ;
#17731 = CARTESIAN_POINT ( 'NONE',  ( 38.93987200065208754, -8.813682088886096722, 70.42958956619168021 ) ) ;
#17732 = ORIENTED_EDGE ( 'NONE', *, *, #12178, .T. ) ;
#17733 = VERTEX_POINT ( 'NONE', #4485 ) ;
#17734 = FACE_OUTER_BOUND ( 'NONE', #7541, .T. ) ;
#17735 = DIRECTION ( 'NONE',  ( 1.734723475976807094E-15, -0.7516416929448819229, -0.6595716529892350355 ) ) ;
#17736 = ORIENTED_EDGE ( 'NONE', *, *, #12405, .T. ) ;
#17737 = DIRECTION ( 'NONE',  ( 0.000000000000000000, -0.6568589528324746407, 0.7540134720837716742 ) ) ;
#17738 = CARTESIAN_POINT ( 'NONE',  ( 39.95015449827720744, -19.00384086642191406, 71.96809898377887293 ) ) ;
#17739 = TOROIDAL_SURFACE ( 'NONE', #11570, 0.9023161253044896801, 0.2000000000000000111 ) ;
#17740 = ADVANCED_FACE ( 'NONE', ( #21875 ), #19943, .F. ) ;
#17741 = LINE ( 'NONE', #20392, #11720 ) ;
#17742 = CARTESIAN_POINT ( 'NONE',  ( 39.02742774030102879, -20.21368208888610241, 72.26730301774234988 ) ) ;
#17743 = EDGE_LOOP ( 'NONE', ( #1169, #10897, #14582, #6098 ) ) ;
#17744 = VECTOR ( 'NONE', #21325, 1000.000000000000000 ) ;
#17745 = VERTEX_POINT ( 'NONE', #340 ) ;
#17746 = DIRECTION ( 'NONE',  ( 0.000000000000000000, -0.7540134720837717852, -0.6568589528324746407 ) ) ;
#17747 = CARTESIAN_POINT ( 'NONE',  ( 39.38009889167650357, -14.21368208888610773, 72.75271321436731853 ) ) ;
#17748 = FACE_OUTER_BOUND ( 'NONE', #12411, .T. ) ;
#17749 = CARTESIAN_POINT ( 'NONE',  ( 43.81606138205700063, -33.60910547091194900, 60.61426200347987248 ) ) ;
#17750 = FACE_OUTER_BOUND ( 'NONE', #8643, .T. ) ;
#17751 = CARTESIAN_POINT ( 'NONE',  ( 17.31606138205699708, 34.87886987267149408, 81.44836866983821722 ) ) ;
#17752 = PRODUCT ( 'Pusher Link Lever', 'Pusher Link Lever', '', ( #3382 ) ) ;
#17753 = PLANE ( 'NONE',  #9455 ) ;
#17754 = EDGE_CURVE ( 'NONE', #21009, #18244, #16441, .T. ) ;
#17755 = ORIENTED_EDGE ( 'NONE', *, *, #2154, .F. ) ;
#17756 = EDGE_CURVE ( 'NONE', #2232, #13035, #20326, .T. ) ;
#17757 = LINE ( 'NONE', #21619, #1638 ) ;
#17758 = VERTEX_POINT ( 'NONE', #16195 ) ;
#17759 = EDGE_CURVE ( 'NONE', #25244, #9104, #4358, .T. ) ;
#17760 = ORIENTED_EDGE ( 'NONE', *, *, #9883, .T. ) ;
#17761 = CIRCLE ( 'NONE', #16925, 4.000000000000000000 ) ;
#17762 = CARTESIAN_POINT ( 'NONE',  ( 40.33642880535521869, -5.303840866421911215, 69.98269868914867686 ) ) ;
#17763 = EDGE_CURVE ( 'NONE', #952, #22308, #24160, .T. ) ;
#17764 = EDGE_CURVE ( 'NONE', #13846, #12986, #17370, .T. ) ;
#17765 = EDGE_LOOP ( 'NONE', ( #7281, #1931, #16801, #9307, #7910 ) ) ;
#17766 = AXIS2_PLACEMENT_3D ( 'NONE', #12145, #19984, #508 ) ;
#17767 = CYLINDRICAL_SURFACE ( 'NONE', #24752, 1.550000000000002709 ) ;
#17768 = CARTESIAN_POINT ( 'NONE',  ( 37.69796330110504101, -11.11368208888610276, 69.66206559358663242 ) ) ;
#17769 = VERTEX_POINT ( 'NONE', #8475 ) ;
#17770 = DIRECTION ( 'NONE',  ( -1.000000000000000000, 0.000000000000000000, 0.000000000000000000 ) ) ;
#17771 = LINE ( 'NONE', #16169, #1791 ) ;
#17772 = ADVANCED_FACE ( 'NONE', ( #2528 ), #10388, .T. ) ;
#17773 = CARTESIAN_POINT ( 'NONE',  ( 40.77203464402485622, -12.51368208888610667, 71.32335560751960202 ) ) ;
#17774 = EDGE_CURVE ( 'NONE', #25151, #9366, #14520, .T. ) ;
#17775 = CYLINDRICAL_SURFACE ( 'NONE', #7766, 0.7500000000000031086 ) ;
#17776 = DIRECTION ( 'NONE',  ( 1.000000000000000000, -5.510910596163088391E-31, -1.836970198721029688E-16 ) ) ;
#17777 = AXIS2_PLACEMENT_3D ( 'NONE', #8674, #18452, #2713 ) ;
#17778 = DIRECTION ( 'NONE',  ( 0.000000000000000000, -0.5706330172266952383, 0.8212051873014186709 ) ) ;
#17779 =( NAMED_UNIT ( * ) PLANE_ANGLE_UNIT ( ) SI_UNIT ( $, .RADIAN. ) );
#17780 = CARTESIAN_POINT ( 'NONE',  ( 36.31606138205702194, -21.37925193044963379, 31.05911325134166034 ) ) ;
#17781 = EDGE_CURVE ( 'NONE', #1739, #18120, #22377, .T. ) ;
#17782 = AXIS2_PLACEMENT_3D ( 'NONE', #4854, #10916, #15026 ) ;
#17783 = CARTESIAN_POINT ( 'NONE',  ( 32.81606138205700773, -22.55876147765401996, 68.80501292737008612 ) ) ;
#17784 = CARTESIAN_POINT ( 'NONE',  ( 37.25260217561390874, -14.00384086642191050, 70.97781676520601479 ) ) ;
#17785 = CARTESIAN_POINT ( 'NONE',  ( 39.24876120206128860, -22.71368208888610241, 70.63227792289245599 ) ) ;
#17786 = VERTEX_POINT ( 'NONE', #16310 ) ;
#17787 = CARTESIAN_POINT ( 'NONE',  ( 38.58006293444520196, -22.20876388569947935, 75.80498974974848636 ) ) ;
#17788 = CARTESIAN_POINT ( 'NONE',  ( 3.816061382056944229, 1.773964314019461419, -3.427682652428185595 ) ) ;
#17789 = VERTEX_POINT ( 'NONE', #4734 ) ;
#17790 = VERTEX_POINT ( 'NONE', #8222 ) ;
#17791 = CARTESIAN_POINT ( 'NONE',  ( 39.64521430340305841, -24.80384086642191832, 73.30173637941817333 ) ) ;
#17792 = CARTESIAN_POINT ( 'NONE',  ( 39.31564783533280405, -22.31368208888609672, 72.03616607671141026 ) ) ;
#17793 = CARTESIAN_POINT ( 'NONE',  ( 38.37017380507020192, -4.013682088886107557, 73.71602215082116061 ) ) ;
#17794 = VECTOR ( 'NONE', #19406, 1000.000000000000000 ) ;
#17795 = ORIENTED_EDGE ( 'NONE', *, *, #4465, .T. ) ;
#17796 = CARTESIAN_POINT ( 'NONE',  ( 33.31606138205700773, -22.22127907754180853, 85.30501292736998664 ) ) ;
#17797 = CIRCLE ( 'NONE', #11216, 2.500000000000002220 ) ;
#17798 = CARTESIAN_POINT ( 'NONE',  ( 38.37017380507018771, -29.60384086642190837, 69.64448340153876416 ) ) ;
#17799 = FACE_OUTER_BOUND ( 'NONE', #22000, .T. ) ;
#17800 = ORIENTED_EDGE ( 'NONE', *, *, #16655, .T. ) ;
#17801 = CARTESIAN_POINT ( 'NONE',  ( 33.56606138205700773, 41.44123852234599070, 73.55501292736987295 ) ) ;
#17802 = CARTESIAN_POINT ( 'NONE',  ( 33.31606138205700773, -5.204193249396356968, 72.80501292736992980 ) ) ;
#17803 = VECTOR ( 'NONE', #6540, 1000.000000000000000 ) ;
#17804 = CARTESIAN_POINT ( 'NONE',  ( 36.11133435605973574, -6.003840866421917610, 70.60699637195612866 ) ) ;
#17805 = DIRECTION ( 'NONE',  ( 1.000000000000000000, 3.217519435284891566E-15, 1.466282614970859239E-16 ) ) ;
#17806 = CARTESIAN_POINT ( 'NONE',  ( 43.31606138205700063, -12.40281258615395465, 20.95421293576468358 ) ) ;
#17807 = CARTESIAN_POINT ( 'NONE',  ( 39.75915168707250302, -12.71368208888610063, 70.26145752964251301 ) ) ;
#17808 = CARTESIAN_POINT ( 'NONE',  ( 36.31606138205700773, -19.47805968271055477, 24.94720442500192448 ) ) ;
#17809 = CIRCLE ( 'NONE', #14920, 1.550000000000002709 ) ;
#17810 = VECTOR ( 'NONE', #728, 1000.000000000000000 ) ;
#17811 = CARTESIAN_POINT ( 'NONE',  ( 37.80618814713140097, -23.91368208888610880, 73.13360434286902034 ) ) ;
#17812 = DIRECTION ( 'NONE',  ( 0.000000000000000000, -0.8212051873014186709, -0.5706330172266952383 ) ) ;
#17813 = ADVANCED_FACE ( 'NONE', ( #6534 ), #485, .T. ) ;
#17814 = CARTESIAN_POINT ( 'NONE',  ( 37.69796330110505522, -2.503840866421913613, 73.09843995877331224 ) ) ;
#17815 = AXIS2_PLACEMENT_3D ( 'NONE', #8341, #4349, #16300 ) ;
#17816 = CARTESIAN_POINT ( 'NONE',  ( 43.31606138205700773, -18.80550481115970740, 25.27912300651437150 ) ) ;
#17817 = CARTESIAN_POINT ( 'NONE',  ( 38.82593461698262871, -20.91368208888609459, 69.62690120949091011 ) ) ;
#17818 = DIRECTION ( 'NONE',  ( 1.000000000000000000, 0.000000000000000000, 0.000000000000000000 ) ) ;
#17819 = AXIS2_PLACEMENT_3D ( 'NONE', #8043, #6732, #17038 ) ;
#17820 = CARTESIAN_POINT ( 'NONE',  ( 38.37017380507018771, -17.60384086642190837, 69.64448340153877837 ) ) ;
#17821 = CARTESIAN_POINT ( 'NONE',  ( 31.91606138205697363, -4.349482454670880571, -5.142398479549302515 ) ) ;
#17822 = AXIS2_PLACEMENT_3D ( 'NONE', #5255, #24548, #856 ) ;
#17823 = CARTESIAN_POINT ( 'NONE',  ( 36.49096545463212493, -11.51368208888609956, 71.43714994484034264 ) ) ;
#17824 = VERTEX_POINT ( 'NONE', #18019 ) ;
#17825 = CARTESIAN_POINT ( 'NONE',  ( 38.37017380507020192, -20.01368208888611022, 73.71602215082113219 ) ) ;
#17826 = EDGE_LOOP ( 'NONE', ( #17645, #681, #1182, #12288 ) ) ;
#17827 = DIRECTION ( 'NONE',  ( 8.758115402030106693E-47, -1.000000000000000000, 3.469446951953613400E-15 ) ) ;
#17828 = CYLINDRICAL_SURFACE ( 'NONE', #10386, 1.249999999999998668 ) ;
#17829 = CARTESIAN_POINT ( 'NONE',  ( 37.89291511884479036, -18.50384086642191406, 72.49843995877330372 ) ) ;
#17830 = ORIENTED_EDGE ( 'NONE', *, *, #21704, .F. ) ;
#17831 = ORIENTED_EDGE ( 'NONE', *, *, #11009, .F. ) ;
#17832 = CARTESIAN_POINT ( 'NONE',  ( 43.81606138205700063, -34.55876147765403061, 66.30501292737011454 ) ) ;
#17833 = CARTESIAN_POINT ( 'NONE',  ( 40.31606138205700773, -13.58280000135113319, 20.54174511886706256 ) ) ;
#17834 = CIRCLE ( 'NONE', #21117, 1.000000000000000888 ) ;
#17835 = CARTESIAN_POINT ( 'NONE',  ( 36.29569395875881099, -22.30384086642192187, 72.77780686321128201 ) ) ;
#17836 = VECTOR ( 'NONE', #24617, 1000.000000000000000 ) ;
#17837 = DIRECTION ( 'NONE',  ( -2.122643018205887308E-17, 1.000000000000000000, -3.120611096041553009E-15 ) ) ;
#17838 = CARTESIAN_POINT ( 'NONE',  ( 39.64521430340304420, -4.813682088886099386, 69.45876917294177133 ) ) ;
#17839 = CARTESIAN_POINT ( 'NONE',  ( 31.81606138205700418, -38.55876147765429351, 66.30501292737328356 ) ) ;
#17840 = EDGE_LOOP ( 'NONE', ( #7433, #5526, #5223, #11354 ) ) ;
#17841 = EDGE_CURVE ( 'NONE', #1958, #13887, #23918, .T. ) ;
#17842 = ORIENTED_EDGE ( 'NONE', *, *, #13010, .T. ) ;
#17843 = EDGE_CURVE ( 'NONE', #5671, #23981, #13259, .T. ) ;
#17844 = CARTESIAN_POINT ( 'NONE',  ( 36.31606138205699352, 5.691238522346996120, 69.09790614618344762 ) ) ;
#17845 = DIRECTION ( 'NONE',  ( 1.000000000000000000, 2.168404344971055214E-16, -1.734723475976814737E-16 ) ) ;
#17846 = AXIS2_PLACEMENT_3D ( 'NONE', #8818, #16657, #3121 ) ;
#17847 = EDGE_CURVE ( 'NONE', #11458, #14769, #12983, .T. ) ;
#17848 = CARTESIAN_POINT ( 'NONE',  ( 38.37017380507018771, -19.60384086642191193, 69.64448340153877837 ) ) ;
#17849 = LINE ( 'NONE', #14231, #7537 ) ;
#17850 = VERTEX_POINT ( 'NONE', #13237 ) ;
#17851 = CARTESIAN_POINT ( 'NONE',  ( 40.31606138205700063, 8.191238522346989015, 65.30501292736998664 ) ) ;
#17852 = CIRCLE ( 'NONE', #3859, 10.00000000000000000 ) ;
#17853 = CARTESIAN_POINT ( 'NONE',  ( 43.31606138205700063, -2.373793412309109563, 19.60611914621674146 ) ) ;
#17854 = ORIENTED_EDGE ( 'NONE', *, *, #25471, .T. ) ;
#17855 = CARTESIAN_POINT ( 'NONE',  ( 37.60469502381300799, -8.403840866421912636, 72.26730301774236409 ) ) ;
#17856 = CARTESIAN_POINT ( 'NONE',  ( 44.81606138205700063, 40.39281886181299797, 66.30501292737000085 ) ) ;
#17857 = ORIENTED_EDGE ( 'NONE', *, *, #3339, .T. ) ;
#17858 = ADVANCED_FACE ( 'NONE', ( #9252 ), #6918, .T. ) ;
#17859 = CIRCLE ( 'NONE', #20319, 1.550000000000002709 ) ;
#17860 = CARTESIAN_POINT ( 'NONE',  ( 43.81606138205700063, -38.55876147765401640, 71.30501292737012875 ) ) ;
#17861 = ORIENTED_EDGE ( 'NONE', *, *, #12176, .T. ) ;
#17862 = VERTEX_POINT ( 'NONE', #7041 ) ;
#17863 = DIRECTION ( 'NONE',  ( 0.000000000000000000, 0.6568589528324745297, -0.7540134720837717852 ) ) ;
#17864 = CARTESIAN_POINT ( 'NONE',  ( 38.00113996487114321, -7.913682088886101695, 72.53360434286905445 ) ) ;
#17865 = CARTESIAN_POINT ( 'NONE',  ( 38.93987200065208754, -4.813682088886099386, 70.42958956619168021 ) ) ;
#17866 = ORIENTED_EDGE ( 'NONE', *, *, #12634, .F. ) ;
#17867 = VERTEX_POINT ( 'NONE', #20571 ) ;
#17868 = LINE ( 'NONE', #17486, #21025 ) ;
#17869 = CARTESIAN_POINT ( 'NONE',  ( 33.31606138205700773, 3.043703737701412226, 64.67489359404071081 ) ) ;
#17870 = ORIENTED_EDGE ( 'NONE', *, *, #6530, .T. ) ;
#17871 = DIRECTION ( 'NONE',  ( -0.000000000000000000, -1.000000000000000000, 2.848211695852029218E-15 ) ) ;
#17872 = CARTESIAN_POINT ( 'NONE',  ( 36.68196826583682935, -20.00384086642191050, 70.79240656858107172 ) ) ;
#17873 = COLOUR_RGB ( '', 0.09019608, 0.27058824, 0.51372549) ;
#17874 = CARTESIAN_POINT ( 'NONE',  ( 43.31606138205700063, -20.55619265724211076, 44.11584019928223910 ) ) ;
#17875 = CARTESIAN_POINT ( 'NONE',  ( 34.56606138205700773, 47.04446929126254417, 81.37823623207319201 ) ) ;
#17876 = DIRECTION ( 'NONE',  ( 1.000000000000000000, -0.000000000000000000, 0.000000000000000000 ) ) ;
#17877 = EDGE_LOOP ( 'NONE', ( #2555, #829, #10859, #7485 ) ) ;
#17878 = VECTOR ( 'NONE', #19794, 1000.000000000000000 ) ;
#17879 = EDGE_LOOP ( 'NONE', ( #3355, #18330, #15059, #18662 ) ) ;
#17880 = CARTESIAN_POINT ( 'NONE',  ( 45.81606138205700063, -21.15876147765410309, 66.30501292737000085 ) ) ;
#17881 = CARTESIAN_POINT ( 'NONE',  ( 36.49096545463212493, -11.51368208888610312, 71.43714994484034264 ) ) ;
#17882 = VECTOR ( 'NONE', #13013, 1000.000000000000000 ) ;
#17883 = DIRECTION ( 'NONE',  ( 1.000000000000000000, -0.000000000000000000, 0.000000000000000000 ) ) ;
#17884 = DIRECTION ( 'NONE',  ( -1.000000000000000000, 1.115179377413661005E-30, 3.717264591378870232E-16 ) ) ;
#17885 = FACE_OUTER_BOUND ( 'NONE', #1639, .T. ) ;
#17886 = DIRECTION ( 'NONE',  ( 1.000000000000000000, 1.115287202090205222E-30, -1.734723475976805122E-15 ) ) ;
#17887 = CARTESIAN_POINT ( 'NONE',  ( 39.31606138205702194, -21.82181003913286332, 31.95585308007613179 ) ) ;
#17888 = CARTESIAN_POINT ( 'NONE',  ( 45.81606138205700063, -38.55876147765399509, 84.30501292737011454 ) ) ;
#17889 = APPLICATION_CONTEXT ( 'automotive_design' ) ;
#17890 = ORIENTED_EDGE ( 'NONE', *, *, #11386, .T. ) ;
#17891 = DIRECTION ( 'NONE',  ( -1.000000000000000000, 1.040834085586084551E-30, 3.469446951953615175E-16 ) ) ;
#17892 = EDGE_CURVE ( 'NONE', #22308, #17597, #12462, .T. ) ;
#17893 = LINE ( 'NONE', #217, #19346 ) ;
#17894 = VERTEX_POINT ( 'NONE', #21087 ) ;
#17895 = ORIENTED_EDGE ( 'NONE', *, *, #13344, .T. ) ;
#17896 = VECTOR ( 'NONE', #22853, 1000.000000000000000 ) ;
#17897 = CARTESIAN_POINT ( 'NONE',  ( 39.73277004305197124, -1.403840866421909972, 69.52238214136768590 ) ) ;
#17898 = ORIENTED_EDGE ( 'NONE', *, *, #17764, .F. ) ;
#17899 = CARTESIAN_POINT ( 'NONE',  ( 43.31606138205700063, -20.93319939328399926, 43.78741072286599945 ) ) ;
#17900 = CARTESIAN_POINT ( 'NONE',  ( 36.49096545463212493, -7.513682088886102228, 71.43714994484035685 ) ) ;
#17901 = ORIENTED_EDGE ( 'NONE', *, *, #16782, .F. ) ;
#17902 = CARTESIAN_POINT ( 'NONE',  ( 44.81606138205700063, -38.55876147765400930, 73.30501292737012875 ) ) ;
#17903 = CARTESIAN_POINT ( 'NONE',  ( 38.26194895904383486, -17.01368208888610312, 69.04448340153878405 ) ) ;
#17904 = EDGE_CURVE ( 'NONE', #126, #2876, #5371, .T. ) ;
#17905 = CARTESIAN_POINT ( 'NONE',  ( 46.81606138205706458, -34.55876147768182705, 70.30501292735635843 ) ) ;
#17906 = DIRECTION ( 'NONE',  ( 0.000000000000000000, 1.000000000000000000, 0.000000000000000000 ) ) ;
#17907 = EDGE_CURVE ( 'NONE', #17225, #4853, #17098, .T. ) ;
#17908 = VECTOR ( 'NONE', #22059, 1000.000000000000000 ) ;
#17909 = CARTESIAN_POINT ( 'NONE',  ( 36.06606138205700063, 6.004618353093779781, 2.291321535809666354 ) ) ;
#17910 = CIRCLE ( 'NONE', #10091, 0.7500000000000021094 ) ;
#17911 = EDGE_CURVE ( 'NONE', #12037, #13486, #24796, .T. ) ;
#17912 =( NAMED_UNIT ( * ) SI_UNIT ( $, .STERADIAN. ) SOLID_ANGLE_UNIT ( ) );
#17913 = DIRECTION ( 'NONE',  ( 0.000000000000000000, -0.8212051873014203363, -0.5706330172266926848 ) ) ;
#17914 = CARTESIAN_POINT ( 'NONE',  ( 40.64099152588522657, 0.3928188618129990761, 83.02501292736999972 ) ) ;
#17915 = DIRECTION ( 'NONE',  ( -1.000000000000000000, 0.000000000000000000, 0.000000000000000000 ) ) ;
#17916 = CARTESIAN_POINT ( 'NONE',  ( 37.60469502381300089, -27.21368208888609885, 70.49320253461758057 ) ) ;
#17917 = EDGE_LOOP ( 'NONE', ( #10637, #2588, #22863, #15776 ) ) ;
#17918 = DIRECTION ( 'NONE',  ( 0.000000000000000000, 2.999999999999999839E-15, 1.000000000000000000 ) ) ;
#17919 = EDGE_CURVE ( 'NONE', #19999, #10282, #7927, .T. ) ;
#17920 = CARTESIAN_POINT ( 'NONE',  ( 43.23147868389327897, 41.43850569188389699, 79.87823623207322044 ) ) ;
#17921 = ORIENTED_EDGE ( 'NONE', *, *, #20873, .T. ) ;
#17922 = ORIENTED_EDGE ( 'NONE', *, *, #199, .T. ) ;
#17923 = CARTESIAN_POINT ( 'NONE',  ( 36.11133435605973574, -26.00384086642192116, 70.60699637195608602 ) ) ;
#17924 = CARTESIAN_POINT ( 'NONE',  ( 38.82593461698262871, -26.91368208888610170, 69.62690120949091011 ) ) ;
#17925 = DIRECTION ( 'NONE',  ( 1.000000000000000000, 0.000000000000000000, 0.000000000000000000 ) ) ;
#17926 = AXIS2_PLACEMENT_3D ( 'NONE', #4761, #13141, #7214 ) ;
#17927 = CARTESIAN_POINT ( 'NONE',  ( 38.00113996487112189, 0.2961591335780902612, 70.22690120949094705 ) ) ;
#17928 = DIRECTION ( 'NONE',  ( 1.000000000000000000, 0.000000000000000000, 0.000000000000000000 ) ) ;
#17929 = EDGE_LOOP ( 'NONE', ( #2959, #23284 ) ) ;
#17930 = LINE ( 'NONE', #8391, #15025 ) ;
#17931 = DIRECTION ( 'NONE',  ( 1.000000000000000000, 2.999999999999999839E-15, 0.000000000000000000 ) ) ;
#17932 = CARTESIAN_POINT ( 'NONE',  ( 39.12911128074872380, -3.503840866421911393, 69.06206559358666652 ) ) ;
#17933 = EDGE_CURVE ( 'NONE', #3377, #5254, #22881, .T. ) ;
#17934 = DIRECTION ( 'NONE',  ( 0.000000000000000000, 2.999999999999999839E-15, 1.000000000000000000 ) ) ;
#17935 = DIRECTION ( 'NONE',  ( -1.000000000000000000, 0.000000000000000000, 0.000000000000000000 ) ) ;
#17936 = CARTESIAN_POINT ( 'NONE',  ( 39.75915168707250302, -4.713682088886100630, 70.26145752964252722 ) ) ;
#17937 = LINE ( 'NONE', #14312, #18361 ) ;
#17938 = EDGE_CURVE ( 'NONE', #3263, #14925, #3038, .T. ) ;
#17939 = CARTESIAN_POINT ( 'NONE',  ( 39.82603832034401847, -28.31368208888610738, 72.40698646996131060 ) ) ;
#17940 = EDGE_CURVE ( 'NONE', #21036, #6661, #22304, .T. ) ;
#17941 = EDGE_CURVE ( 'NONE', #12862, #15888, #3168, .T. ) ;
#17942 = DIRECTION ( 'NONE',  ( -1.734723475976804876E-16, 1.000000000000000000, 3.009265538105065326E-32 ) ) ;
#17943 = CARTESIAN_POINT ( 'NONE',  ( 37.25202387243754032, -0.4038408664219159117, 72.75271321436733274 ) ) ;
#17944 = PLANE ( 'NONE',  #7142 ) ;
#17945 = CARTESIAN_POINT ( 'NONE',  ( 37.12184278917507640, -28.10384086642191193, 71.32335560751960202 ) ) ;
#17946 = CARTESIAN_POINT ( 'NONE',  ( 36.49096545463212493, -9.513682088886101340, 71.43714994484035685 ) ) ;
#17947 = LINE ( 'NONE', #19868, #24224 ) ;
#17948 = EDGE_CURVE ( 'NONE', #6765, #22555, #12508, .T. ) ;
#17949 = CARTESIAN_POINT ( 'NONE',  ( 37.80618814713138676, -9.703840866421904465, 69.62690120949091011 ) ) ;
#17950 = DIRECTION ( 'NONE',  ( 0.000000000000000000, -1.000000000000000000, 4.382459307730880209E-15 ) ) ;
#17951 = CARTESIAN_POINT ( 'NONE',  ( 38.82593461698262871, -14.91368208888609637, 69.62690120949091011 ) ) ;
#17952 = ORIENTED_EDGE ( 'NONE', *, *, #15156, .T. ) ;
#17953 = CARTESIAN_POINT ( 'NONE',  ( 39.64521430340304420, -18.81368208888610027, 69.45876917294175712 ) ) ;
#17954 = VERTEX_POINT ( 'NONE', #18896 ) ;
#17955 = DIRECTION ( 'NONE',  ( -0.000000000000000000, -3.469446951953613400E-15, -1.000000000000000000 ) ) ;
#17956 = DIRECTION ( 'NONE',  ( 0.000000000000000000, -0.4425581086832361399, 0.8967398287344645613 ) ) ;
#17957 = CARTESIAN_POINT ( 'NONE',  ( 39.41296390513587511, -17.20384086642191335, 71.08074471024441721 ) ) ;
#17958 = VERTEX_POINT ( 'NONE', #22627 ) ;
#17959 = ADVANCED_FACE ( 'NONE', ( #18638 ), #18767, .F. ) ;
#17960 = EDGE_LOOP ( 'NONE', ( #3673, #17002, #2780, #21100 ) ) ;
#17961 = PLANE ( 'NONE',  #16639 ) ;
#17962 = DIRECTION ( 'NONE',  ( -6.464932690748116116E-17, -0.1431355622335914179, 0.9897030922575081879 ) ) ;
#17963 = CARTESIAN_POINT ( 'NONE',  ( 36.98690846071097127, -19.80384086642191477, 69.45876917294175712 ) ) ;
#17964 = CARTESIAN_POINT ( 'NONE',  ( 36.31606138205700063, 38.69123852234599781, 75.30501292737004349 ) ) ;
#17965 = CARTESIAN_POINT ( 'NONE',  ( 39.98359781491296161, -28.41368208888610525, 71.86517103874045631 ) ) ;
#17966 = PRODUCT_DEFINITION_SHAPE ( 'NONE', 'NONE',  #9653 ) ;
#17967 = DIRECTION ( 'NONE',  ( -0.000000000000000000, -3.469446951953613400E-15, -1.000000000000000000 ) ) ;
#17968 = EDGE_LOOP ( 'NONE', ( #16763, #11870, #3547, #13855 ) ) ;
#17969 = FACE_OUTER_BOUND ( 'NONE', #8774, .T. ) ;
#17970 = DIRECTION ( 'NONE',  ( -1.000000000000000000, 1.040834085586084551E-30, 3.469446951953615175E-16 ) ) ;
#17971 = CARTESIAN_POINT ( 'NONE',  ( 38.37017380507018771, -21.60384086642190837, 69.64448340153877837 ) ) ;
#17972 = FACE_OUTER_BOUND ( 'NONE', #363, .T. ) ;
#17973 = EDGE_LOOP ( 'NONE', ( #6055, #17712, #6654, #21722 ) ) ;
#17974 = CARTESIAN_POINT ( 'NONE',  ( 39.81746892067405952, 41.43850569188389699, 79.37823623207322044 ) ) ;
#17975 = CARTESIAN_POINT ( 'NONE',  ( 42.96606138205697789, -6.230354416574639842, -1.331254207427787328 ) ) ;
#17976 = CARTESIAN_POINT ( 'NONE',  ( 39.41296390513587511, 0.7961591335780872081, 71.08074471024443142 ) ) ;
#17977 = CARTESIAN_POINT ( 'NONE',  ( 44.81606138205700063, 1.441238522345976714, 67.80501292737001506 ) ) ;
#17978 = ORIENTED_EDGE ( 'NONE', *, *, #23684, .T. ) ;
#17979 = CARTESIAN_POINT ( 'NONE',  ( 39.75915168707250302, -28.71368208888609175, 70.26145752964249880 ) ) ;
#17980 = EDGE_LOOP ( 'NONE', ( #3521, #3304, #7467, #9776 ) ) ;
#17981 = ORIENTED_EDGE ( 'NONE', *, *, #21733, .F. ) ;
#17982 = CARTESIAN_POINT ( 'NONE',  ( 32.81606138205700773, -38.55876147765401640, 70.30501292737012875 ) ) ;
#17984 = EDGE_CURVE ( 'NONE', #2290, #3395, #8988, .T. ) ;
#17983 = CYLINDRICAL_SURFACE ( 'NONE', #2983, 0.5000000000000004441 ) ;
#17985 = UNCERTAINTY_MEASURE_WITH_UNIT (LENGTH_MEASURE( 1.000000000000000082E-05 ), #4006, 'distance_accuracy_value', 'NONE');
#17986 = CARTESIAN_POINT ( 'NONE',  ( 38.73920764526925353, -8.113682088886099208, 72.49843995877331793 ) ) ;
#17987 = EDGE_CURVE ( 'NONE', #13184, #10377, #19026, .T. ) ;
#17988 = CARTESIAN_POINT ( 'NONE',  ( 37.25260217561390874, -3.613682088886100097, 71.78268878715394408 ) ) ;
#17989 = ORIENTED_EDGE ( 'NONE', *, *, #10191, .T. ) ;
#17990 = ORIENTED_EDGE ( 'NONE', *, *, #3960, .T. ) ;
#17991 = DIRECTION ( 'NONE',  ( -6.938893903907229955E-15, -1.000000000000000000, 2.999999999999999839E-15 ) ) ;
#17992 = DIRECTION ( 'NONE',  ( 0.000000000000000000, -1.000000000000000000, 2.999999999999999839E-15 ) ) ;
#17993 = ORIENTED_EDGE ( 'NONE', *, *, #8713, .T. ) ;
#17994 = CARTESIAN_POINT ( 'NONE',  ( 41.14099152588522657, -10.60718113818700026, 83.30501292737001506 ) ) ;
#17995 = CARTESIAN_POINT ( 'NONE',  ( 40.14115730948191185, -9.103840866421911926, 71.43714994484034264 ) ) ;
#17996 = VECTOR ( 'NONE', #18617, 1000.000000000000000 ) ;
#17997 = CIRCLE ( 'NONE', #18807, 2.500000000000002220 ) ;
#17998 = VECTOR ( 'NONE', #24500, 1000.000000000000000 ) ;
#17999 = CARTESIAN_POINT ( 'NONE',  ( 36.32862050049384806, -20.56764888167150929, 75.95432206938126285 ) ) ;
#18000 = DIRECTION ( 'NONE',  ( -0.1733269559585479680, -3.077057697073492856E-15, -0.9848643390529192576 ) ) ;
#18001 = ORIENTED_EDGE ( 'NONE', *, *, #18059, .F. ) ;
#18002 = ORIENTED_EDGE ( 'NONE', *, *, #7695, .T. ) ;
#18003 = DIRECTION ( 'NONE',  ( -1.836970198721029688E-16, -2.999999999999999839E-15, -1.000000000000000000 ) ) ;
#18004 = CARTESIAN_POINT ( 'NONE',  ( 37.25202387243752611, -9.213682088886100630, 70.00779233799264034 ) ) ;
#18005 = EDGE_CURVE ( 'NONE', #10314, #2590, #12253, .T. ) ;
#18006 = CARTESIAN_POINT ( 'NONE',  ( 43.81606138205700063, -0.03546393544221274063, 20.62209909563275900 ) ) ;
#18007 = DIRECTION ( 'NONE',  ( 0.000000000000000000, 0.9814242980364923374, 0.1918498038142812112 ) ) ;
#18008 = DIRECTION ( 'NONE',  ( 0.000000000000000000, 3.469446951953611033E-15, 1.000000000000000000 ) ) ;
#18009 = PLANE ( 'NONE',  #24996 ) ;
#18010 = VECTOR ( 'NONE', #11619, 1000.000000000000000 ) ;
#18011 = CARTESIAN_POINT ( 'NONE',  ( 45.81606138205700063, -36.05876147765410877, 70.30501292737000085 ) ) ;
#18012 = CARTESIAN_POINT ( 'NONE',  ( 36.31606138205700063, 5.691238522346989903, 65.80501292736998664 ) ) ;
#18013 = VECTOR ( 'NONE', #23866, 1000.000000000000000 ) ;
#18014 = AXIS2_PLACEMENT_3D ( 'NONE', #17729, #1607, #7944 ) ;
#18015 = EDGE_LOOP ( 'NONE', ( #19211, #5610, #10903, #6758, #13079, #1290, #12964, #15506, #11431, #5126, #23380, #1589 ) ) ;
#18016 = CARTESIAN_POINT ( 'NONE',  ( 40.31606138205700773, -29.06829118875199924, 75.30501292737000085 ) ) ;
#18017 = EDGE_LOOP ( 'NONE', ( #7976, #3669, #1208, #8115, #11676, #1245, #21304, #25027, #21948, #25391, #19702, #1719 ) ) ;
#18018 = ORIENTED_EDGE ( 'NONE', *, *, #20283, .F. ) ;
#18019 = CARTESIAN_POINT ( 'NONE',  ( 43.81606138205700063, 41.44123852234599070, 73.55501292736987295 ) ) ;
#18020 = PRODUCT_DEFINITION_CONTEXT ( 'detailed design', #15233, 'design' ) ;
#18021 = CARTESIAN_POINT ( 'NONE',  ( 40.52078840805429394, -3.003840866421914502, 72.15350918040385864 ) ) ;
#18022 = ADVANCED_FACE ( 'NONE', ( #11689 ), #5743, .F. ) ;
#18023 = ORIENTED_EDGE ( 'NONE', *, *, #24650, .T. ) ;
#18024 = DIRECTION ( 'NONE',  ( -1.734723475976814737E-16, 1.000000000000000000, -3.491481338843135327E-15 ) ) ;
#18025 = CARTESIAN_POINT ( 'NONE',  ( 37.33957961208646736, -7.813682088886109156, 72.81632618279323310 ) ) ;
#18026 = VERTEX_POINT ( 'NONE', #17345 ) ;
#18027 = DIRECTION ( 'NONE',  ( 1.000000000000000000, 0.000000000000000000, 0.000000000000000000 ) ) ;
#18028 = CARTESIAN_POINT ( 'NONE',  ( 39.64521430340304420, -12.81368208888610383, 69.45876917294175712 ) ) ;
#18029 = AXIS2_PLACEMENT_3D ( 'NONE', #2273, #10027, #24154 ) ;
#18030 = DIRECTION ( 'NONE',  ( -1.327674326049719602E-15, 0.4425581086832399147, -0.8967398287344627850 ) ) ;
#18031 = AXIS2_PLACEMENT_3D ( 'NONE', #9521, #19045, #9768 ) ;
#18032 = CARTESIAN_POINT ( 'NONE',  ( 39.81606138205699352, 2.191238522346989015, 65.80501292737000085 ) ) ;
#18033 = EDGE_CURVE ( 'NONE', #25120, #13976, #13734, .T. ) ;
#18034 = ORIENTED_EDGE ( 'NONE', *, *, #6702, .F. ) ;
#18035 = CARTESIAN_POINT ( 'NONE',  ( 45.06606138205707879, -39.99575152356565155, 63.13209164280871022 ) ) ;
#18036 = CARTESIAN_POINT ( 'NONE',  ( 44.81606138205700063, 40.39281886181299797, 84.30501292736984453 ) ) ;
#18037 = PLANE ( 'NONE',  #15371 ) ;
#18038 = FACE_BOUND ( 'NONE', #468, .T. ) ;
#18039 = CARTESIAN_POINT ( 'NONE',  ( 37.21915885897815457, -25.41368208888610170, 71.08074471024441721 ) ) ;
#18040 = VERTEX_POINT ( 'NONE', #15278 ) ;
#18041 = CARTESIAN_POINT ( 'NONE',  ( 46.81606138205707168, -36.80651332587431313, 65.82119181171029254 ) ) ;
#18042 = DIRECTION ( 'NONE',  ( -1.000000000000000000, -3.083952846180990083E-15, 9.251858538542970050E-30 ) ) ;
#18043 = ORIENTED_EDGE ( 'NONE', *, *, #9517, .F. ) ;
#18044 = VERTEX_POINT ( 'NONE', #60 ) ;
#18045 = CARTESIAN_POINT ( 'NONE',  ( 38.26194895904384197, -26.60384086642191903, 73.71602215082113219 ) ) ;
#18046 = CIRCLE ( 'NONE', #10226, 1.249999999999998890 ) ;
#18047 = CARTESIAN_POINT ( 'NONE',  ( 36.87297107704152666, -27.71368208888610241, 72.49904802271738902 ) ) ;
#18048 = LINE ( 'NONE', #4266, #2486 ) ;
#18049 = DIRECTION ( 'NONE',  ( -1.000000000000000000, 0.000000000000000000, 0.000000000000000000 ) ) ;
#18050 = ORIENTED_EDGE ( 'NONE', *, *, #13287, .T. ) ;
#18051 = DIRECTION ( 'NONE',  ( 2.690219486203388234E-15, -0.8967398287344627850, -0.4425581086832399147 ) ) ;
#18052 = DIRECTION ( 'NONE',  ( 1.000000000000000000, 3.469446951953611033E-15, 0.000000000000000000 ) ) ;
#18053 = CARTESIAN_POINT ( 'NONE',  ( 36.89935272106205133, -2.403840866421917521, 73.23812341099225875 ) ) ;
#18054 = PRESENTATION_LAYER_ASSIGNMENT (  '', '', ( #20939 ) ) ;
#18055 = PLANE ( 'NONE',  #1643 ) ;
#18056 = FACE_OUTER_BOUND ( 'NONE', #23637, .T. ) ;
#18057 = CARTESIAN_POINT ( 'NONE',  ( 39.95015449827720744, -6.613682088886106314, 70.79240656858107172 ) ) ;
#18058 = DIRECTION ( 'NONE',  ( -2.452751524064188892E-15, 1.000000000000000000, 0.000000000000000000 ) ) ;
#18059 = EDGE_CURVE ( 'NONE', #2190, #15969, #23127, .T. ) ;
#18060 = CARTESIAN_POINT ( 'NONE',  ( 39.83125377402841139, -28.67593286074587411, 70.46188669365974988 ) ) ;
#18061 = AXIS2_PLACEMENT_3D ( 'NONE', #20279, #18729, #24119 ) ;
#18062 = CARTESIAN_POINT ( 'NONE',  ( 36.31606138205702194, -20.02093502212016318, 26.61211107664843212 ) ) ;
#18063 = DIRECTION ( 'NONE',  ( 0.000000000000000000, -0.8212051873014208914, -0.5706330172266919076 ) ) ;
#18064 = ITEM_DEFINED_TRANSFORMATION ( 'NONE', 'NONE', #14573,  #2000 ) ;
#18065 = CARTESIAN_POINT ( 'NONE',  ( 43.31606138205700063, -13.58280000135112964, 20.54174511886706256 ) ) ;
#18066 = VECTOR ( 'NONE', #9418, 1000.000000000000000 ) ;
#18067 = CARTESIAN_POINT ( 'NONE',  ( 37.25260217561390874, -28.00384086642191406, 70.97781676520601479 ) ) ;
#18068 = CARTESIAN_POINT ( 'NONE',  ( 37.69796330110504101, -13.11368208888609743, 69.66206559358661821 ) ) ;
#18069 = DIRECTION ( 'NONE',  ( 0.000000000000000000, -0.3299742535180970049, 0.9439899321577400748 ) ) ;
#18070 = AXIS2_PLACEMENT_3D ( 'NONE', #9010, #13001, #11063 ) ;
#18071 = CARTESIAN_POINT ( 'NONE',  ( 36.80608444377001831, -10.30384086642191654, 72.40698646996136745 ) ) ;
#18072 = EDGE_CURVE ( 'NONE', #12220, #12767, #11940, .T. ) ;
#18073 = DIRECTION ( 'NONE',  ( -1.000000000000000000, 0.000000000000000000, 0.000000000000000000 ) ) ;
#18074 = EDGE_CURVE ( 'NONE', #18554, #13035, #13477, .T. ) ;
#18075 = CARTESIAN_POINT ( 'NONE',  ( 36.68196826583682935, -9.613682088886104538, 71.96809898377890136 ) ) ;
#18076 = ORIENTED_EDGE ( 'NONE', *, *, #11208, .T. ) ;
#18077 = CARTESIAN_POINT ( 'NONE',  ( 40.33642880535524000, -18.31368208888610383, 72.77780686321126780 ) ) ;
#18078 = ORIENTED_EDGE ( 'NONE', *, *, #17282, .T. ) ;
#18079 = LINE ( 'NONE', #12546, #15628 ) ;
#18080 = EDGE_CURVE ( 'NONE', #12198, #20897, #9871, .T. ) ;
#18081 = DIRECTION ( 'NONE',  ( 1.327674326049719602E-15, -0.4425581086832399147, 0.8967398287344627850 ) ) ;
#18082 = CARTESIAN_POINT ( 'NONE',  ( 37.12184278917507640, -18.10384086642191193, 71.32335560751961623 ) ) ;
#18083 = ADVANCED_FACE ( 'NONE', ( #25041, #25169 ), #1731, .T. ) ;
#18084 = EDGE_CURVE ( 'NONE', #6775, #16347, #17599, .T. ) ;
#18085 = AXIS2_PLACEMENT_3D ( 'NONE', #21137, #5548, #13286 ) ;
#18086 = EDGE_LOOP ( 'NONE', ( #842, #12519, #14809, #16268, #3220 ) ) ;
#18087 = VERTEX_POINT ( 'NONE', #15788 ) ;
#18088 = CARTESIAN_POINT ( 'NONE',  ( 42.96606138205697789, -5.898435835062210586, -2.003809078978638247 ) ) ;
#18089 = LINE ( 'NONE', #18337, #9204 ) ;
#18090 = CARTESIAN_POINT ( 'NONE',  ( 37.50301148336529877, -24.50384086642192116, 73.69843995877326392 ) ) ;
#18091 = DIRECTION ( 'NONE',  ( 1.000000000000000000, 0.000000000000000000, 0.000000000000000000 ) ) ;
#18092 = CARTESIAN_POINT ( 'NONE',  ( 40.55423172469004811, 1.586317911113896306, 72.05058123536544201 ) ) ;
#18093 = LINE ( 'NONE', #8170, #21308 ) ;
#18094 = EDGE_CURVE ( 'NONE', #13492, #22911, #23644, .T. ) ;
#18095 = AXIS2_PLACEMENT_3D ( 'NONE', #10276, #334, #8346 ) ;
#18096 = EDGE_LOOP ( 'NONE', ( #6797, #16315, #10670, #6306 ) ) ;
#18097 = VECTOR ( 'NONE', #10798, 1000.000000000000000 ) ;
#18098 = CARTESIAN_POINT ( 'NONE',  ( 33.48992690894276336, 2.908530785145326814, 6.098665089938691608 ) ) ;
#18099 = CARTESIAN_POINT ( 'NONE',  ( 33.56606138205700773, 41.44123852234599781, 74.30501292736987295 ) ) ;
#18100 = CARTESIAN_POINT ( 'NONE',  ( 37.69796330110505522, -18.50384086642191406, 73.09843995877329803 ) ) ;
#18101 = CARTESIAN_POINT ( 'NONE',  ( 31.56606138205697576, -4.349482454670882348, -5.142398479549302515 ) ) ;
#18102 = AXIS2_PLACEMENT_3D ( 'NONE', #7067, #14919, #24825 ) ;
#18103 = EDGE_LOOP ( 'NONE', ( #16370, #23579, #12824, #8648 ) ) ;
#18104 = CARTESIAN_POINT ( 'NONE',  ( 36.31606138205700063, -11.51539968388052060, 18.41550321377400934 ) ) ;
#18105 = EDGE_CURVE ( 'NONE', #23863, #5367, #23506, .T. ) ;
#18106 = DIRECTION ( 'NONE',  ( 3.053249489819422104E-16, 0.5703958094953464064, 0.8213699656732943444 ) ) ;
#18107 = CARTESIAN_POINT ( 'NONE',  ( 39.41296390513587511, -1.203840866421910905, 71.08074471024443142 ) ) ;
#18108 = CIRCLE ( 'NONE', #6562, 0.9023161253044892360 ) ;
#18109 = CYLINDRICAL_SURFACE ( 'NONE', #2443, 0.5000000000000004441 ) ;
#18110 = VERTEX_POINT ( 'NONE', #17480 ) ;
#18111 = CARTESIAN_POINT ( 'NONE',  ( 32.81606138205700773, 41.44123852234599070, 73.30501292736987295 ) ) ;
#18112 = ORIENTED_EDGE ( 'NONE', *, *, #16571, .F. ) ;
#18113 = VERTEX_POINT ( 'NONE', #7562 ) ;
#18114 = LINE ( 'NONE', #8572, #7403 ) ;
#18115 = CARTESIAN_POINT ( 'NONE',  ( 43.81606138205700063, 46.72314894770294558, 81.17823623207318917 ) ) ;
#18116 = CIRCLE ( 'NONE', #7423, 0.5000000000000011102 ) ;
#18117 = CARTESIAN_POINT ( 'NONE',  ( 38.73920764526925353, -4.113682088886099208, 72.49843995877331793 ) ) ;
#18118 = CARTESIAN_POINT ( 'NONE',  ( 39.37952058850012804, -6.613682088886101873, 70.97781676520601479 ) ) ;
#18119 = ORIENTED_EDGE ( 'NONE', *, *, #3981, .F. ) ;
#18120 = VERTEX_POINT ( 'NONE', #6004 ) ;
#18121 = DIRECTION ( 'NONE',  ( 1.000000000000000000, 1.156482317317870344E-15, 0.000000000000000000 ) ) ;
#18122 = CARTESIAN_POINT ( 'NONE',  ( 43.81606138205700063, 35.12314894770293705, 81.37823623207324886 ) ) ;
#18123 = CARTESIAN_POINT ( 'NONE',  ( 40.81606138205700773, -29.37462871496113337, 53.20604314849776983 ) ) ;
#18124 = CARTESIAN_POINT ( 'NONE',  ( 39.82603832034400426, -13.30384086642190233, 70.35351908239857721 ) ) ;
#18125 = DIRECTION ( 'NONE',  ( 0.000000000000000000, 0.4425581086832403033, -0.8967398287344625629 ) ) ;
#18126 = CYLINDRICAL_SURFACE ( 'NONE', #18407, 1.750000000000001776 ) ;
#18127 = ORIENTED_EDGE ( 'NONE', *, *, #7202, .T. ) ;
#18128 = EDGE_LOOP ( 'NONE', ( #7476, #23381, #5584, #7182, #18418, #9486, #23096, #23643, #24560, #18879, #11750 ) ) ;
#18129 = ORIENTED_EDGE ( 'NONE', *, *, #8300, .T. ) ;
#18130 = LINE ( 'NONE', #19799, #5479 ) ;
#18131 = VECTOR ( 'NONE', #6980, 1000.000000000000000 ) ;
#18132 = CARTESIAN_POINT ( 'NONE',  ( 36.68196826583682935, -9.613682088886104538, 71.96809898377890136 ) ) ;
#18133 = CARTESIAN_POINT ( 'NONE',  ( 41.96606138205694236, 6.548188142891450347, 4.975198841308384523 ) ) ;
#18134 = DIRECTION ( 'NONE',  ( 0.000000000000000000, 1.000000000000000000, -2.999999999999999839E-15 ) ) ;
#18135 = AXIS2_PLACEMENT_3D ( 'NONE', #1889, #25199, #5904 ) ;
#18136 = CARTESIAN_POINT ( 'NONE',  ( 35.64099152588523367, -0.6071811381869983704, 122.0250129273699997 ) ) ;
#18137 = DIRECTION ( 'NONE',  ( 0.000000000000000000, -0.3299742535180970049, 0.9439899321577400748 ) ) ;
#18138 = ADVANCED_FACE ( 'NONE', ( #21208 ), #13857, .F. ) ;
#18139 = ADVANCED_FACE ( 'NONE', ( #15525 ), #13362, .T. ) ;
#18140 = DIRECTION ( 'NONE',  ( 2.792262043613788535E-15, -0.8967398287344627850, -0.4425581086832399147 ) ) ;
#18141 = CARTESIAN_POINT ( 'NONE',  ( 44.06606138205700063, 40.39281886181299797, 84.30501292736984453 ) ) ;
#18142 = LINE ( 'NONE', #14017, #4952 ) ;
#18143 = ORIENTED_EDGE ( 'NONE', *, *, #25442, .T. ) ;
#18144 = VERTEX_POINT ( 'NONE', #19650 ) ;
#18145 = DIRECTION ( 'NONE',  ( 0.000000000000000000, 1.000000000000000000, 0.000000000000000000 ) ) ;
#18146 = CARTESIAN_POINT ( 'NONE',  ( 40.26954217208372455, -4.903840866421919742, 72.86986841596736042 ) ) ;
#18147 = AXIS2_PLACEMENT_3D ( 'NONE', #7949, #570, #949 ) ;
#18148 = ORIENTED_EDGE ( 'NONE', *, *, #19631, .F. ) ;
#18149 = DIRECTION ( 'NONE',  ( 1.734723475976814737E-16, 0.000000000000000000, 1.000000000000000000 ) ) ;
#18150 = CARTESIAN_POINT ( 'NONE',  ( 36.49096545463212493, -5.513682088886105781, 71.43714994484035685 ) ) ;
#18151 = AXIS2_PLACEMENT_3D ( 'NONE', #24005, #2494, #17726 ) ;
#18152 = CARTESIAN_POINT ( 'NONE',  ( 43.31606138205700063, -5.204193249396356968, 72.80501292736992980 ) ) ;
#18153 = CARTESIAN_POINT ( 'NONE',  ( 36.89935272106204422, -17.21368208888610241, 69.52238214136768590 ) ) ;
#18154 = LINE ( 'NONE', #11988, #17646 ) ;
#18155 = FACE_OUTER_BOUND ( 'NONE', #5146, .T. ) ;
#18156 = EDGE_CURVE ( 'NONE', #12466, #10938, #713, .T. ) ;
#18157 = CARTESIAN_POINT ( 'NONE',  ( 43.27366112336382287, 3.802330592292169964, 6.334870612574754034 ) ) ;
#18158 = ADVANCED_FACE ( 'NONE', ( #19270 ), #21459, .T. ) ;
#18159 = CARTESIAN_POINT ( 'NONE',  ( 33.31606138205700773, 2.715274261285174351, 65.05190033008260286 ) ) ;
#18160 = EDGE_CURVE ( 'NONE', #18110, #9433, #23377, .T. ) ;
#18161 = PLANE ( 'NONE',  #23963 ) ;
#18162 = VECTOR ( 'NONE', #8076, 1000.000000000000000 ) ;
#18163 = CARTESIAN_POINT ( 'NONE',  ( 44.81606138205700063, -38.55876147765404482, 61.30501292737012164 ) ) ;
#18164 = CARTESIAN_POINT ( 'NONE',  ( 39.37952058850012804, -24.61368208888610454, 70.97781676520600058 ) ) ;
#18165 = SHAPE_REPRESENTATION ( 'Pusher Link Lever', ( #2000 ), #7588 ) ;
#18166 = ORIENTED_EDGE ( 'NONE', *, *, #15223, .T. ) ;
#18167 = CARTESIAN_POINT ( 'NONE',  ( 30.81606138205700418, -33.05876147765410167, 70.30501292737000085 ) ) ;
#18168 = LINE ( 'NONE', #15959, #2894 ) ;
#18169 = ORIENTED_EDGE ( 'NONE', *, *, #20456, .T. ) ;
#18170 = VERTEX_POINT ( 'NONE', #2796 ) ;
#18171 = CARTESIAN_POINT ( 'NONE',  ( 39.73277004305197124, -21.40384086642191619, 69.52238214136768590 ) ) ;
#18172 = EDGE_CURVE ( 'NONE', #4506, #4432, #16852, .T. ) ;
#18173 = PRODUCT_DEFINITION_SHAPE ( 'NONE', 'NONE',  #25489 ) ;
#18174 = CARTESIAN_POINT ( 'NONE',  ( 36.68196826583682935, -27.61368208888610809, 71.96809898377887293 ) ) ;
#18175 = FACE_OUTER_BOUND ( 'NONE', #17401, .T. ) ;
#18176 = DIRECTION ( 'NONE',  ( 1.000000000000000000, 6.505213034913019208E-17, -1.734723475976809806E-16 ) ) ;
#18177 = LINE ( 'NONE', #22151, #16813 ) ;
#18178 = ORIENTED_EDGE ( 'NONE', *, *, #11569, .T. ) ;
#18179 = CARTESIAN_POINT ( 'NONE',  ( 38.31606138205700063, -5.204193249396280585, 82.80501292736992980 ) ) ;
#18180 = CARTESIAN_POINT ( 'NONE',  ( 32.81606138205700773, -34.55876147765707174, 70.30501292736873609 ) ) ;
#18181 = CARTESIAN_POINT ( 'NONE',  ( 36.29569395875881099, -4.303840866421919209, 72.77780686321129622 ) ) ;
#18182 = DIRECTION ( 'NONE',  ( 2.412663730047099099E-15, -0.8967398287344627850, -0.4425581086832399147 ) ) ;
#18183 = CARTESIAN_POINT ( 'NONE',  ( 46.81606138205695089, 5.290470704224636833, -0.3848988112044732235 ) ) ;
#18184 = CARTESIAN_POINT ( 'NONE',  ( 37.25202387243752611, -9.213682088886100630, 70.00779233799264034 ) ) ;
#18185 = CARTESIAN_POINT ( 'NONE',  ( 43.23147868389327897, 42.38065457974295924, 79.52109337493037344 ) ) ;
#18186 = DIRECTION ( 'NONE',  ( 0.000000000000000000, 0.8191520442889929088, 0.5735764363510444941 ) ) ;
#18187 = DIRECTION ( 'NONE',  ( 7.071067811865491110E-16, -0.9008287146801832179, 0.4341746501209495790 ) ) ;
#18188 = ITEM_DEFINED_TRANSFORMATION ( 'NONE', 'NONE', #12540,  #2000 ) ;
#18189 = CARTESIAN_POINT ( 'NONE',  ( 43.24580177837434292, 3.721690752961227755, 6.335617458560805382 ) ) ;
#18190 = CARTESIAN_POINT ( 'NONE',  ( 37.31647492878124694, -26.30384086642190766, 72.03616607671141026 ) ) ;
#18191 = CARTESIAN_POINT ( 'NONE',  ( 37.69796330110504101, -11.11368208888610276, 69.66206559358663242 ) ) ;
#18192 = CARTESIAN_POINT ( 'NONE',  ( 33.63983381732847988, 3.338985100189466149, 6.348312178689456964 ) ) ;
#18193 = AXIS2_PLACEMENT_3D ( 'NONE', #17292, #16771, #6853 ) ;
#18194 = VECTOR ( 'NONE', #12224, 1000.000000000000000 ) ;
#18195 = CARTESIAN_POINT ( 'NONE',  ( 37.69796330110505522, -14.50384086642191583, 73.09843995877329803 ) ) ;
#18196 = FACE_OUTER_BOUND ( 'NONE', #19233, .T. ) ;
#18197 = EDGE_CURVE ( 'NONE', #17183, #21390, #5138, .T. ) ;
#18198 = AXIS2_PLACEMENT_3D ( 'NONE', #843, #20443, #24419 ) ;
#18199 = CARTESIAN_POINT ( 'NONE',  ( 39.29254315202756231, -8.813682088886100274, 69.94417936956673998 ) ) ;
#18200 = EDGE_LOOP ( 'NONE', ( #25284, #3490, #20717, #5125 ) ) ;
#18201 = CARTESIAN_POINT ( 'NONE',  ( 35.86008812008917346, -13.51368208888610667, 71.43714994484034264 ) ) ;
#18202 = ORIENTED_EDGE ( 'NONE', *, *, #12854, .F. ) ;
#18203 = CARTESIAN_POINT ( 'NONE',  ( 31.81606138205700418, 0.1601050959395486362, 68.80395113470939350 ) ) ;
#18204 = CARTESIAN_POINT ( 'NONE',  ( 38.31606138205700063, 15.19123852234700500, 71.30501292736995822 ) ) ;
#18205 = CARTESIAN_POINT ( 'NONE',  ( 39.24876120206129571, -16.90384086642190553, 72.12822762946747446 ) ) ;
#18206 = ORIENTED_EDGE ( 'NONE', *, *, #3717, .F. ) ;
#18207 = VERTEX_POINT ( 'NONE', #20721 ) ;
#18208 = DIRECTION ( 'NONE',  ( 0.000000000000000000, -1.000000000000000000, 2.999999999999999839E-15 ) ) ;
#18209 = FACE_OUTER_BOUND ( 'NONE', #1423, .T. ) ;
#18210 = CARTESIAN_POINT ( 'NONE',  ( 40.26954217208372455, -22.90384086642191974, 72.86986841596734621 ) ) ;
#18211 = CARTESIAN_POINT ( 'NONE',  ( 32.81606138205700773, 35.12314894770294416, 81.17823623207323180 ) ) ;
#18212 = CARTESIAN_POINT ( 'NONE',  ( 39.75915168707250302, -28.71368208888609175, 70.26145752964249880 ) ) ;
#18213 = DIRECTION ( 'NONE',  ( 0.000000000000000000, -0.4425581086832404143, 0.8967398287344625629 ) ) ;
#18214 = VECTOR ( 'NONE', #22648, 1000.000000000000000 ) ;
#18215 = ORIENTED_EDGE ( 'NONE', *, *, #4239, .F. ) ;
#18216 = ORIENTED_EDGE ( 'NONE', *, *, #23406, .F. ) ;
#18217 = CARTESIAN_POINT ( 'NONE',  ( 36.31606138205700063, -31.05876147765399864, 75.30501292737010033 ) ) ;
#18218 = EDGE_CURVE ( 'NONE', #15078, #9125, #22116, .T. ) ;
#18219 = CARTESIAN_POINT ( 'NONE',  ( 42.68042513965293949, 15.19123852234700323, 70.30501292736995822 ) ) ;
#18220 = AXIS2_PLACEMENT_3D ( 'NONE', #9879, #9506, #9756 ) ;
#18221 = CARTESIAN_POINT ( 'NONE',  ( 36.49096545463212493, -12.10384086642191193, 71.32335560751961623 ) ) ;
#18222 = EDGE_CURVE ( 'NONE', #6167, #12702, #23334, .T. ) ;
#18223 = CARTESIAN_POINT ( 'NONE',  ( 33.31606138205700773, -5.204193249396356968, 72.80501292736992980 ) ) ;
#18224 = ADVANCED_FACE ( 'NONE', ( #20341 ), #18781, .T. ) ;
#18225 = CARTESIAN_POINT ( 'NONE',  ( 33.31606138205700773, 3.536347952325769040, 64.10938348997790115 ) ) ;
#18226 = AXIS2_PLACEMENT_3D ( 'NONE', #23551, #11472, #2040 ) ;
#18227 = VECTOR ( 'NONE', #4492, 1000.000000000000000 ) ;
#18228 = CYLINDRICAL_SURFACE ( 'NONE', #4934, 0.7499999999999983347 ) ;
#18229 = CARTESIAN_POINT ( 'NONE',  ( 36.64852494920107517, -28.20384086642191335, 71.86517103874047052 ) ) ;
#18230 = DIRECTION ( 'NONE',  ( -1.000000000000000000, -3.083952846180990083E-15, 9.251858538542970050E-30 ) ) ;
#18231 = ORIENTED_EDGE ( 'NONE', *, *, #15206, .T. ) ;
#18232 = ADVANCED_FACE ( 'NONE', ( #22263 ), #24434, .F. ) ;
#18233 = CIRCLE ( 'NONE', #8784, 1.500000000000001332 ) ;
#18234 = CARTESIAN_POINT ( 'NONE',  ( 33.31606138205700773, 7.187001342539796944, 66.09667597968754649 ) ) ;
#18235 = ORIENTED_EDGE ( 'NONE', *, *, #5767, .F. ) ;
#18236 = ORIENTED_EDGE ( 'NONE', *, *, #13741, .F. ) ;
#18237 = DIRECTION ( 'NONE',  ( -1.000000000000000000, -2.999999999999999839E-15, 0.000000000000000000 ) ) ;
#18238 = VECTOR ( 'NONE', #18885, 1000.000000000000000 ) ;
#18239 = CARTESIAN_POINT ( 'NONE',  ( 41.81606138205687273, 43.19123852234595518, 61.80501292736988006 ) ) ;
#18240 = UNCERTAINTY_MEASURE_WITH_UNIT (LENGTH_MEASURE( 1.000000000000000082E-05 ), #19502, 'distance_accuracy_value', 'NONE');
#18241 = CARTESIAN_POINT ( 'NONE',  ( 37.69225076346193504, -5.813682088886100274, 72.33091598616827866 ) ) ;
#18242 = CARTESIAN_POINT ( 'NONE',  ( 39.24876120206128860, -6.713682088886101518, 70.63227792289247020 ) ) ;
#18243 = ORIENTED_EDGE ( 'NONE', *, *, #4369, .T. ) ;
#18244 = VERTEX_POINT ( 'NONE', #24174 ) ;
#18245 = CARTESIAN_POINT ( 'NONE',  ( 43.81606138205700063, -1.963190818658398173, 19.89143565483009013 ) ) ;
#18246 = CIRCLE ( 'NONE', #7127, 1.000000000000000888 ) ;
#18247 = CARTESIAN_POINT ( 'NONE',  ( 31.81606138205700418, 38.19123852234599070, 73.05501292736988717 ) ) ;
#18248 = CARTESIAN_POINT ( 'NONE',  ( 33.31606138205700773, -35.82531359714782582, 71.25150419970752580 ) ) ;
#18249 = CARTESIAN_POINT ( 'NONE',  ( 38.37017380507018771, -9.603840866421908373, 69.64448340153879258 ) ) ;
#18250 = VECTOR ( 'NONE', #17746, 1000.000000000000227 ) ;
#18251 = DIRECTION ( 'NONE',  ( -2.122643018205887308E-17, 1.000000000000000000, -3.120611096041553009E-15 ) ) ;
#18252 = EDGE_LOOP ( 'NONE', ( #5432, #7290, #9339, #8379 ) ) ;
#18253 = ORIENTED_EDGE ( 'NONE', *, *, #21926, .T. ) ;
#18254 = ORIENTED_EDGE ( 'NONE', *, *, #20187, .T. ) ;
#18255 = DIRECTION ( 'NONE',  ( 0.000000000000000000, -0.6568589528324746407, 0.7540134720837716742 ) ) ;
#18256 = CARTESIAN_POINT ( 'NONE',  ( 36.64852494920107517, -7.413682088886104360, 70.89533451361948835 ) ) ;
#18257 = CARTESIAN_POINT ( 'NONE',  ( 33.81606138205700063, 16.19123852234703520, 80.30501292736995822 ) ) ;
#18258 = AXIS2_PLACEMENT_3D ( 'NONE', #22964, #24877, #3248 ) ;
#18259 = DIRECTION ( 'NONE',  ( 1.000000000000000000, 0.000000000000000000, 0.000000000000000000 ) ) ;
#18260 = EDGE_CURVE ( 'NONE', #24890, #17540, #9792, .T. ) ;
#18261 = EDGE_CURVE ( 'NONE', #5671, #4880, #7060, .T. ) ;
#18262 = ORIENTED_EDGE ( 'NONE', *, *, #25301, .F. ) ;
#18263 = CARTESIAN_POINT ( 'NONE',  ( 36.80608444377001121, -23.31368208888610383, 70.35351908239857721 ) ) ;
#18264 = CARTESIAN_POINT ( 'NONE',  ( 43.31606138205700063, -35.70002751211045933, 71.94742330197156832 ) ) ;
#18265 = VECTOR ( 'NONE', #19339, 1000.000000000000114 ) ;
#18266 = FACE_OUTER_BOUND ( 'NONE', #21264, .T. ) ;
#18267 = DIRECTION ( 'NONE',  ( -1.000000000000000000, 0.000000000000000000, 0.000000000000000000 ) ) ;
#18268 = CIRCLE ( 'NONE', #13320, 1.499999999999996669 ) ;
#18269 = EDGE_CURVE ( 'NONE', #18272, #9258, #20846, .T. ) ;
#18270 = DIRECTION ( 'NONE',  ( -2.412663730047099099E-15, 0.8967398287344627850, 0.4425581086832399147 ) ) ;
#18271 = ORIENTED_EDGE ( 'NONE', *, *, #11580, .F. ) ;
#18272 = VERTEX_POINT ( 'NONE', #10553 ) ;
#18273 = DIRECTION ( 'NONE',  ( -0.000000000000000000, -3.469446951953613400E-15, -1.000000000000000000 ) ) ;
#18274 = CARTESIAN_POINT ( 'NONE',  ( 36.36258059203030513, -1.903840866421910638, 69.89063713639259845 ) ) ;
#18275 = CARTESIAN_POINT ( 'NONE',  ( 38.63098279924288647, -22.91368208888609814, 70.22690120949090442 ) ) ;
#18276 = VERTEX_POINT ( 'NONE', #14787 ) ;
#18277 = ORIENTED_EDGE ( 'NONE', *, *, #16777, .T. ) ;
#18278 = DIRECTION ( 'NONE',  ( 0.000000000000000000, 1.000000000000000000, 0.000000000000000000 ) ) ;
#18279 = CARTESIAN_POINT ( 'NONE',  ( 36.68196826583682935, -11.61368208888610276, 71.96809898377888715 ) ) ;
#18280 = VECTOR ( 'NONE', #22016, 1000.000000000000000 ) ;
#18281 = AXIS2_PLACEMENT_3D ( 'NONE', #18685, #6831, #14813 ) ;
#18282 = DIRECTION ( 'NONE',  ( 0.000000000000000000, -0.5706330172266919076, 0.8212051873014208914 ) ) ;
#18283 = EDGE_CURVE ( 'NONE', #2367, #18444, #16588, .T. ) ;
#18284 = AXIS2_PLACEMENT_3D ( 'NONE', #10387, #575, #15130 ) ;
#18285 = CARTESIAN_POINT ( 'NONE',  ( 39.64521430340304420, -6.813682088886101162, 69.45876917294177133 ) ) ;
#18286 = CARTESIAN_POINT ( 'NONE',  ( 42.99533221766311897, 2.835194994361335485, 6.100154078057893337 ) ) ;
#18287 = CARTESIAN_POINT ( 'NONE',  ( 38.41621794735363693, -35.10729675983900222, 83.30501292737010033 ) ) ;
#18288 = CARTESIAN_POINT ( 'NONE',  ( 33.31606138205700773, -5.204193249396280585, 82.80501292736992980 ) ) ;
#18289 = PRODUCT_DEFINITION_FORMATION_WITH_SPECIFIED_SOURCE ( 'ANY', '', #7662, .NOT_KNOWN. ) ;
#18290 = DIRECTION ( 'NONE',  ( 1.000000000000000000, 0.000000000000000000, 0.000000000000000000 ) ) ;
#18291 = AXIS2_PLACEMENT_3D ( 'NONE', #22441, #20259, #6602 ) ;
#18292 = LINE ( 'NONE', #24528, #24028 ) ;
#18293 = CARTESIAN_POINT ( 'NONE',  ( 42.56606138205700063, -39.60075215179220720, 69.23691647014479145 ) ) ;
#18294 = ORIENTED_EDGE ( 'NONE', *, *, #24517, .F. ) ;
#18295 = CARTESIAN_POINT ( 'NONE',  ( 40.11656585159207822, -21.10117404812173802, 75.36211584159703136 ) ) ;
#18296 = VECTOR ( 'NONE', #9849, 1000.000000000000000 ) ;
#18297 = FACE_OUTER_BOUND ( 'NONE', #22686, .T. ) ;
#18298 = ORIENTED_EDGE ( 'NONE', *, *, #17843, .F. ) ;
#18299 = ORIENTED_EDGE ( 'NONE', *, *, #23741, .T. ) ;
#18300 = CARTESIAN_POINT ( 'NONE',  ( 39.64521430340305841, -22.80384086642191832, 73.30173637941818754 ) ) ;
#18301 = CARTESIAN_POINT ( 'NONE',  ( 39.75915168707250302, -28.71368208888609175, 70.26145752964249880 ) ) ;
#18302 = LINE ( 'NONE', #8384, #13619 ) ;
#18303 = EDGE_CURVE ( 'NONE', #8101, #4612, #16457, .T. ) ;
#18304 = ADVANCED_FACE ( 'NONE', ( #4871, #22646, #14410 ), #8879, .F. ) ;
#18305 = FACE_OUTER_BOUND ( 'NONE', #4212, .T. ) ;
#18306 = DIRECTION ( 'NONE',  ( 1.000000000000000000, -1.115179377413661005E-30, -3.717264591378870232E-16 ) ) ;
#18307 = VERTEX_POINT ( 'NONE', #4622 ) ;
#18308 = DIRECTION ( 'NONE',  ( -5.047295537021760406E-31, 1.000000000000000000, -3.491481338843135327E-15 ) ) ;
#18309 = EDGE_CURVE ( 'NONE', #7627, #11457, #11270, .T. ) ;
#18310 = CARTESIAN_POINT ( 'NONE',  ( 36.31606138205700063, -13.04008168869994932, 21.66778101221729713 ) ) ;
#18311 = CARTESIAN_POINT ( 'NONE',  ( 36.89935272106205133, -4.403840866421918854, 73.23812341099225875 ) ) ;
#18312 = DIRECTION ( 'NONE',  ( 0.000000000000000000, 0.5706330172266920187, -0.8212051873014210024 ) ) ;
#18313 = LINE ( 'NONE', #761, #9567 ) ;
#18314 = CARTESIAN_POINT ( 'NONE',  ( 37.80618814713140097, -7.913682088886107913, 73.13360434286904876 ) ) ;
#18315 = PLANE ( 'NONE',  #6397 ) ;
#18316 = CARTESIAN_POINT ( 'NONE',  ( 37.33957961208646736, -19.81368208888611093, 72.81632618279321889 ) ) ;
#18317 =( BOUNDED_CURVE ( )  B_SPLINE_CURVE ( 3, ( #13602, #19018, #19520, #21452 ),
 .UNSPECIFIED., .F., .T. ) 
 B_SPLINE_CURVE_WITH_KNOTS ( ( 4, 4 ),
 ( 1.794712260653050184E-16, 1.570796326794901221 ),
 .UNSPECIFIED. ) 
 CURVE ( )  GEOMETRIC_REPRESENTATION_ITEM ( )  RATIONAL_B_SPLINE_CURVE ( ( 1.000000000000000000, 0.8047378541243640493, 0.8047378541243640493, 1.000000000000000000 ) ) 
 REPRESENTATION_ITEM ( '' )  );
#18318 = DIRECTION ( 'NONE',  ( 0.000000000000000000, -0.4425581086832348077, 0.8967398287344653385 ) ) ;
#18319 = EDGE_CURVE ( 'NONE', #5929, #3431, #17178, .T. ) ;
#18320 = DIRECTION ( 'NONE',  ( -1.000000000000000000, 0.000000000000000000, 0.000000000000000000 ) ) ;
#18321 = CARTESIAN_POINT ( 'NONE',  ( 37.12184278917507640, -24.10384086642191193, 71.32335560751960202 ) ) ;
#18322 = CARTESIAN_POINT ( 'NONE',  ( 39.29254315202756231, -10.81368208888610205, 69.94417936956673998 ) ) ;
#18323 = DIRECTION ( 'NONE',  ( -2.602085213965212219E-15, 0.8967398287344632291, 0.4425581086832389155 ) ) ;
#18324 = EDGE_LOOP ( 'NONE', ( #5119, #16040, #5422, #10852, #8072, #23901, #2813, #7145, #6354, #18477, #6256, #20908 ) ) ;
#18325 = CARTESIAN_POINT ( 'NONE',  ( 40.14115730948191185, -13.10384086642191015, 71.43714994484030001 ) ) ;
#18326 = CARTESIAN_POINT ( 'NONE',  ( 43.31606138205700063, -39.23120981750657421, 69.49370132789680099 ) ) ;
#18327 = CARTESIAN_POINT ( 'NONE',  ( 39.29254315202756231, -6.813682088886101162, 69.94417936956673998 ) ) ;
#18328 = ORIENTED_EDGE ( 'NONE', *, *, #17022, .F. ) ;
#18329 = CARTESIAN_POINT ( 'NONE',  ( 40.26954217208371034, -16.71368208888610241, 69.89063713639258424 ) ) ;
#18330 = ORIENTED_EDGE ( 'NONE', *, *, #5989, .T. ) ;
#18331 = FACE_OUTER_BOUND ( 'NONE', #68, .T. ) ;
#18332 = LINE ( 'NONE', #24222, #7083 ) ;
#18333 = CARTESIAN_POINT ( 'NONE',  ( 38.37017380507018771, -19.60384086642191193, 70.24448340153875847 ) ) ;
#18334 = ORIENTED_EDGE ( 'NONE', *, *, #12729, .T. ) ;
#18335 = ORIENTED_EDGE ( 'NONE', *, *, #23086, .T. ) ;
#18336 = DIRECTION ( 'NONE',  ( -1.000000000000000000, -1.000000000000000078E-15, 0.000000000000000000 ) ) ;
#18337 = CARTESIAN_POINT ( 'NONE',  ( 41.81606138205700063, -20.93319939328399926, 43.78741072286599945 ) ) ;
#18338 = CARTESIAN_POINT ( 'NONE',  ( 40.77203464402485622, -25.10384086642191903, 71.43714994484031422 ) ) ;
#18339 = FACE_OUTER_BOUND ( 'NONE', #19160, .T. ) ;
#18340 = CARTESIAN_POINT ( 'NONE',  ( 36.80608444377001121, -25.31368208888610383, 70.35351908239857721 ) ) ;
#18341 = DIRECTION ( 'NONE',  ( 1.734723475976804876E-16, 3.491481338843135327E-15, 1.000000000000000000 ) ) ;
#18342 = CARTESIAN_POINT ( 'NONE',  ( 36.31606138205700063, -10.66749763588700262, 14.47455635838400134 ) ) ;
#18343 = ORIENTED_EDGE ( 'NONE', *, *, #16178, .F. ) ;
#18344 = DIRECTION ( 'NONE',  ( -1.000000000000000000, -6.197457809535974789E-17, -1.134781633102316229E-16 ) ) ;
#18345 = DIRECTION ( 'NONE',  ( -0.000000000000000000, 0.5735764363510447161, -0.8191520442889929088 ) ) ;
#18346 = EDGE_CURVE ( 'NONE', #24769, #3808, #10932, .T. ) ;
#18347 = CARTESIAN_POINT ( 'NONE',  ( 37.25202387243754032, -14.40384086642191619, 72.75271321436731853 ) ) ;
#18348 = CARTESIAN_POINT ( 'NONE',  ( 0.000000000000000000, 0.000000000000000000, 0.000000000000000000 ) ) ;
#18349 = FACE_OUTER_BOUND ( 'NONE', #12069, .T. ) ;
#18350 = DIRECTION ( 'NONE',  ( -1.000000000000000000, -1.000000000000000078E-15, 0.000000000000000000 ) ) ;
#18351 = DIRECTION ( 'NONE',  ( -1.000000000000000000, -2.999999999999999839E-15, 0.000000000000000000 ) ) ;
#18352 = CARTESIAN_POINT ( 'NONE',  ( 39.24876120206129571, -0.9038408664219128585, 72.12822762946750288 ) ) ;
#18353 = CARTESIAN_POINT ( 'NONE',  ( 44.06606138205700063, 40.39281886181299797, 84.30501292736984453 ) ) ;
#18354 = ORIENTED_EDGE ( 'NONE', *, *, #1385, .T. ) ;
#18355 = CARTESIAN_POINT ( 'NONE',  ( 39.95015449827720744, -26.61368208888610809, 70.79240656858104330 ) ) ;
#18356 = ORIENTED_EDGE ( 'NONE', *, *, #15151, .F. ) ;
#18357 = ORIENTED_EDGE ( 'NONE', *, *, #1826, .F. ) ;
#18358 = CARTESIAN_POINT ( 'NONE',  ( 33.56606138205700773, -36.55876147765401640, 71.30501292737011454 ) ) ;
#18359 = PLANE ( 'NONE',  #21918 ) ;
#18360 = CARTESIAN_POINT ( 'NONE',  ( 37.60469502381300089, -3.213682088886101962, 70.49320253461759478 ) ) ;
#18361 = VECTOR ( 'NONE', #12147, 1000.000000000000227 ) ;
#18362 = CARTESIAN_POINT ( 'NONE',  ( 38.63098279924288647, -6.913682088886101695, 70.22690120949091863 ) ) ;
#18363 = VERTEX_POINT ( 'NONE', #22770 ) ;
#18364 = ORIENTED_EDGE ( 'NONE', *, *, #19571, .T. ) ;
#18365 = DIRECTION ( 'NONE',  ( 1.327674326049719602E-15, -0.4425581086832399147, 0.8967398287344627850 ) ) ;
#18366 = CYLINDRICAL_SURFACE ( 'NONE', #20680, 2.000000000000001776 ) ;
#18367 = CARTESIAN_POINT ( 'NONE',  ( 39.98359781491296161, -13.20384086642191157, 70.89533451361945993 ) ) ;
#18368 = PRESENTATION_STYLE_ASSIGNMENT (( #20421 ) ) ;
#18369 = CARTESIAN_POINT ( 'NONE',  ( 33.31606138205700773, 3.536347952325769040, 64.10938348997790115 ) ) ;
#18370 = ORIENTED_EDGE ( 'NONE', *, *, #15120, .T. ) ;
#18371 = VERTEX_POINT ( 'NONE', #10800 ) ;
#18372 = EDGE_LOOP ( 'NONE', ( #12907, #2430 ) ) ;
#18373 = CARTESIAN_POINT ( 'NONE',  ( 44.81606138205700063, -38.55876147765410167, 70.30501292737011454 ) ) ;
#18374 = CARTESIAN_POINT ( 'NONE',  ( 40.14115730948191185, -8.513682088886106669, 71.32335560751961623 ) ) ;
#18375 = ADVANCED_FACE ( 'NONE', ( #995, #18655, #7582, #9518 ), #7194, .T. ) ;
#18376 = LINE ( 'NONE', #18257, #4039 ) ;
#18377 = CARTESIAN_POINT ( 'NONE',  ( 38.31606138205700773, -22.27515649656512053, 29.48506754039017963 ) ) ;
#18378 = LINE ( 'NONE', #8594, #16381 ) ;
#18379 = LINE ( 'NONE', #22747, #25477 ) ;
#18380 = LINE ( 'NONE', #4603, #13898 ) ;
#18381 = CYLINDRICAL_SURFACE ( 'NONE', #11550, 1.999999999999999556 ) ;
#18382 = ORIENTED_EDGE ( 'NONE', *, *, #24899, .F. ) ;
#18383 = VERTEX_POINT ( 'NONE', #3561 ) ;
#18384 = VECTOR ( 'NONE', #14254, 1000.000000000000227 ) ;
#18385 = DIRECTION ( 'NONE',  ( 0.000000000000000000, 0.000000000000000000, 1.000000000000000000 ) ) ;
#18386 = CARTESIAN_POINT ( 'NONE',  ( 35.86008812008917346, -27.51368208888610667, 71.43714994484032843 ) ) ;
#18387 = EDGE_CURVE ( 'NONE', #18958, #16794, #15425, .T. ) ;
#18388 = VECTOR ( 'NONE', #13554, 1000.000000000000227 ) ;
#18389 = VECTOR ( 'NONE', #8148, 1000.000000000000000 ) ;
#18390 = EDGE_CURVE ( 'NONE', #20720, #1537, #20463, .T. ) ;
#18391 = CARTESIAN_POINT ( 'NONE',  ( 37.60469502381300089, -25.21368208888610241, 70.49320253461758057 ) ) ;
#18392 = ORIENTED_EDGE ( 'NONE', *, *, #15703, .F. ) ;
#18393 = VERTEX_POINT ( 'NONE', #13626 ) ;
#18394 = CARTESIAN_POINT ( 'NONE',  ( 43.81606138205700063, 38.19123852234599070, 72.05501292736988717 ) ) ;
#18395 = CARTESIAN_POINT ( 'NONE',  ( 38.82593461698262871, -2.913682088886099919, 69.62690120949091011 ) ) ;
#18396 = CARTESIAN_POINT ( 'NONE',  ( 38.93415946300896024, -27.50384086642189985, 69.66206559358660400 ) ) ;
#18397 = EDGE_CURVE ( 'NONE', #17105, #7712, #21102, .T. ) ;
#18398 = EDGE_CURVE ( 'NONE', #8601, #19706, #23747, .T. ) ;
#18399 = EDGE_CURVE ( 'NONE', #13201, #4779, #5633, .T. ) ;
#18400 = CARTESIAN_POINT ( 'NONE',  ( 30.81606138205698286, -4.589472609077252407, -6.350807634294811876 ) ) ;
#18401 = CARTESIAN_POINT ( 'NONE',  ( 36.11133435605973574, -5.613682088886105426, 72.15350918040385864 ) ) ;
#18402 = CARTESIAN_POINT ( 'NONE',  ( 42.90907157547642470, 3.273800194542833442, 6.355715097685992632 ) ) ;
#18403 = DIRECTION ( 'NONE',  ( -1.734723475976804876E-16, -3.491481338843135327E-15, -1.000000000000000000 ) ) ;
#18404 = EDGE_CURVE ( 'NONE', #9681, #17658, #3449, .T. ) ;
#18405 = AXIS2_PLACEMENT_3D ( 'NONE', #20904, #21660, #17677 ) ;
#18406 = DIRECTION ( 'NONE',  ( 0.000000000000000000, -0.1999999999999926281, 0.9797958971132726402 ) ) ;
#18407 = AXIS2_PLACEMENT_3D ( 'NONE', #451, #16049, #15921 ) ;
#18408 = EDGE_CURVE ( 'NONE', #21396, #6643, #13122, .T. ) ;
#18409 = CARTESIAN_POINT ( 'NONE',  ( 43.31606138205700063, 4.103895195095678794, 6.341006091748962348 ) ) ;
#18410 = VECTOR ( 'NONE', #18187, 1000.000000000000227 ) ;
#18411 = AXIS2_PLACEMENT_3D ( 'NONE', #24549, #2918, #6672 ) ;
#18412 = FACE_OUTER_BOUND ( 'NONE', #19525, .T. ) ;
#18413 = LINE ( 'NONE', #15834, #24214 ) ;
#18414 = ORIENTED_EDGE ( 'NONE', *, *, #14602, .F. ) ;
#18415 = CARTESIAN_POINT ( 'NONE',  ( 39.20536636138601949, -22.01751967489730077, 75.30696121124701392 ) ) ;
#18416 = CARTESIAN_POINT ( 'NONE',  ( 34.06606138205700773, -32.75315594507191008, 59.38245422252773409 ) ) ;
#18417 = ORIENTED_EDGE ( 'NONE', *, *, #14230, .F. ) ;
#18418 = ORIENTED_EDGE ( 'NONE', *, *, #13971, .F. ) ;
#18419 = CARTESIAN_POINT ( 'NONE',  ( 40.52078840805429394, -17.00384086642191406, 72.15350918040381600 ) ) ;
#18420 = CARTESIAN_POINT ( 'NONE',  ( 37.69796330110504101, -25.11368208888609388, 69.66206559358660400 ) ) ;
#18421 = CARTESIAN_POINT ( 'NONE',  ( 43.81606138205700063, -2.088476903695762665, 19.19551655256602984 ) ) ;
#18422 = VECTOR ( 'NONE', #6609, 1000.000000000000114 ) ;
#18423 = VECTOR ( 'NONE', #16692, 1000.000000000000000 ) ;
#18424 = DIRECTION ( 'NONE',  ( -1.000000000000000000, 0.000000000000000000, 0.000000000000000000 ) ) ;
#18425 = LINE ( 'NONE', #12518, #24600 ) ;
#18426 = ORIENTED_EDGE ( 'NONE', *, *, #25366, .T. ) ;
#18427 = DIRECTION ( 'NONE',  ( 0.000000000000000000, 0.4278636397681519488, -0.9038432971286278761 ) ) ;
#18428 = DIRECTION ( 'NONE',  ( 1.000000000000000000, 0.000000000000000000, 0.000000000000000000 ) ) ;
#18429 = CARTESIAN_POINT ( 'NONE',  ( 40.77203464402485622, -26.51368208888610667, 71.32335560751960202 ) ) ;
#18430 = DIRECTION ( 'NONE',  ( -1.000000000000000000, 0.000000000000000000, 0.000000000000000000 ) ) ;
#18431 = LINE ( 'NONE', #20108, #9963 ) ;
#18432 = CARTESIAN_POINT ( 'NONE',  ( 39.82603832034400426, -10.31368208888610383, 72.40698646996135324 ) ) ;
#18433 = FACE_OUTER_BOUND ( 'NONE', #5968, .T. ) ;
#18434 = CARTESIAN_POINT ( 'NONE',  ( 39.29254315202756231, -18.81368208888610027, 69.94417936956672577 ) ) ;
#18435 = CARTESIAN_POINT ( 'NONE',  ( 39.64097644196145609, -21.75010033615993876, 75.81628532166148204 ) ) ;
#18436 = CIRCLE ( 'NONE', #2369, 0.4999999999999943379 ) ;
#18437 = ADVANCED_FACE ( 'NONE', ( #9647 ), #25187, .T. ) ;
#18438 = DIRECTION ( 'NONE',  ( 1.000000000000000000, 0.000000000000000000, 0.000000000000000000 ) ) ;
#18439 = CARTESIAN_POINT ( 'NONE',  ( 38.63098279924290068, -26.70384086642191690, 72.53360434286901182 ) ) ;
#18440 = CARTESIAN_POINT ( 'NONE',  ( 37.69796330110504101, -15.11368208888609743, 69.66206559358661821 ) ) ;
#18441 = CIRCLE ( 'NONE', #23766, 1.000000000000000888 ) ;
#18442 = ORIENTED_EDGE ( 'NONE', *, *, #14287, .T. ) ;
#18443 = DIRECTION ( 'NONE',  ( -1.000000000000000000, -1.734723475976804876E-16, 1.734723475976814737E-16 ) ) ;
#18444 = VERTEX_POINT ( 'NONE', #24930 ) ;
#18445 = CARTESIAN_POINT ( 'NONE',  ( 38.26194895904384907, -8.603840866421915479, 73.11602215082118050 ) ) ;
#18446 = DIRECTION ( 'NONE',  ( 0.000000000000000000, 3.469446951953613400E-15, 1.000000000000000000 ) ) ;
#18447 = CARTESIAN_POINT ( 'NONE',  ( 39.82603832034400426, -4.313682088886107380, 72.40698646996135324 ) ) ;
#18448 = ORIENTED_EDGE ( 'NONE', *, *, #8636, .F. ) ;
#18449 = CARTESIAN_POINT ( 'NONE',  ( 37.61123632939165873, -13.91368208888610525, 73.73360434286898624 ) ) ;
#18450 = VERTEX_POINT ( 'NONE', #7315 ) ;
#18451 = LINE ( 'NONE', #16255, #14403 ) ;
#18452 = DIRECTION ( 'NONE',  ( -1.000000000000000000, -1.000000000000000078E-15, 0.000000000000000000 ) ) ;
#18453 = CARTESIAN_POINT ( 'NONE',  ( 37.69225076346193504, -13.80384086642191122, 70.42958956619168021 ) ) ;
#18454 = DIRECTION ( 'NONE',  ( 0.000000000000000000, 0.4425581086832403033, -0.8967398287344625629 ) ) ;
#18455 = EDGE_LOOP ( 'NONE', ( #6288, #14322, #9592, #25310 ) ) ;
#18456 = PLANE ( 'NONE',  #12940 ) ;
#18457 = PLANE ( 'NONE',  #17819 ) ;
#18458 = CARTESIAN_POINT ( 'NONE',  ( 37.50301148336529877, -16.50384086642191761, 73.69843995877327814 ) ) ;
#18459 = DIRECTION ( 'NONE',  ( -1.734723475976814737E-16, 1.000000000000000000, -3.491481338843135327E-15 ) ) ;
#18460 = CARTESIAN_POINT ( 'NONE',  ( 37.80618814713140097, -23.91368208888610880, 73.13360434286902034 ) ) ;
#18461 = CARTESIAN_POINT ( 'NONE',  ( 42.96606138205697789, -5.898435835062210586, -2.003809078978638247 ) ) ;
#18462 = DIRECTION ( 'NONE',  ( 1.000000000000000000, 8.911169920151748851E-16, 3.114923731923493702E-16 ) ) ;
#18463 = CIRCLE ( 'NONE', #8191, 1.000000000000012657 ) ;
#18464 = ORIENTED_EDGE ( 'NONE', *, *, #109, .T. ) ;
#18465 = DIRECTION ( 'NONE',  ( 0.000000000000000000, -0.3299742535180970049, 0.9439899321577400748 ) ) ;
#18466 = FACE_OUTER_BOUND ( 'NONE', #19372, .T. ) ;
#18467 = CARTESIAN_POINT ( 'NONE',  ( 37.33957961208645315, -17.80384086642190766, 69.94417936956672577 ) ) ;
#18468 = CARTESIAN_POINT ( 'NONE',  ( 0.000000000000000000, 0.000000000000000000, 0.000000000000000000 ) ) ;
#18469 = EDGE_CURVE ( 'NONE', #19510, #5267, #21345, .T. ) ;
#18470 = DIRECTION ( 'NONE',  ( -1.000000000000000000, 0.000000000000000000, 0.000000000000000000 ) ) ;
#18471 = VECTOR ( 'NONE', #23810, 1000.000000000000227 ) ;
#18472 = EDGE_CURVE ( 'NONE', #24795, #536, #9385, .T. ) ;
#18473 = CARTESIAN_POINT ( 'NONE',  ( 33.66606138205694521, 5.208890205473720059, 5.429380561359602453 ) ) ;
#18474 = LINE ( 'NONE', #14603, #5364 ) ;
#18475 = CARTESIAN_POINT ( 'NONE',  ( 37.33957961208645315, -27.80384086642191122, 69.94417936956671156 ) ) ;
#18476 = CARTESIAN_POINT ( 'NONE',  ( 38.31606138205700063, -29.30876147765400930, 72.30501292737010033 ) ) ;
#18477 = ORIENTED_EDGE ( 'NONE', *, *, #23645, .F. ) ;
#18478 = VECTOR ( 'NONE', #17179, 1000.000000000000000 ) ;
#18479 = CARTESIAN_POINT ( 'NONE',  ( 36.64852494920107517, -27.41368208888610525, 70.89533451361945993 ) ) ;
#18480 = VERTEX_POINT ( 'NONE', #5383 ) ;
#18481 = ORIENTED_EDGE ( 'NONE', *, *, #19713, .T. ) ;
#18482 = CARTESIAN_POINT ( 'NONE',  ( 42.71151723894909225, 2.752945995551776992, 6.094624432592374852 ) ) ;
#18483 = CARTESIAN_POINT ( 'NONE',  ( 31.81606138205700418, 18.19123852234598715, 71.05501292736995822 ) ) ;
#18484 = CARTESIAN_POINT ( 'NONE',  ( 39.24876120206129571, -28.90384086642191264, 72.12822762946746025 ) ) ;
#18485 = AXIS2_PLACEMENT_3D ( 'NONE', #22110, #4350, #2269 ) ;
#18486 = CARTESIAN_POINT ( 'NONE',  ( 39.51027997493896748, 1.486317911113900658, 71.32335560751961623 ) ) ;
#18487 = VERTEX_POINT ( 'NONE', #11707 ) ;
#18488 = EDGE_LOOP ( 'NONE', ( #7295, #1138, #20854, #19124 ) ) ;
#18489 = CARTESIAN_POINT ( 'NONE',  ( 33.33836326447716658, 3.869514117107255569, 6.310928887378282504 ) ) ;
#18490 = ADVANCED_FACE ( 'NONE', ( #13251 ), #15291, .T. ) ;
#18491 = DIRECTION ( 'NONE',  ( 9.925461516413221718E-16, -0.8967398287344632291, -0.4425581086832394151 ) ) ;
#18492 = EDGE_LOOP ( 'NONE', ( #1620, #4193, #10437, #9155 ) ) ;
#18493 = DIRECTION ( 'NONE',  ( 0.000000000000000000, 0.9992330079037401447, -0.03915859951076000600 ) ) ;
#18494 = CARTESIAN_POINT ( 'NONE',  ( 40.14115730948191185, -13.10384086642191015, 71.43714994484030001 ) ) ;
#18495 = VECTOR ( 'NONE', #1757, 1000.000000000000000 ) ;
#18496 = DIRECTION ( 'NONE',  ( 1.734723475976807094E-15, -0.7516416929448819229, -0.6595716529892350355 ) ) ;
#18497 = ORIENTED_EDGE ( 'NONE', *, *, #23804, .F. ) ;
#18498 = ORIENTED_EDGE ( 'NONE', *, *, #14050, .F. ) ;
#18499 = VECTOR ( 'NONE', #13158, 1000.000000000000227 ) ;
#18500 = DIRECTION ( 'NONE',  ( 1.734723475976804876E-16, 3.252606517456515274E-15, 1.000000000000000000 ) ) ;
#18501 = CARTESIAN_POINT ( 'NONE',  ( 39.95015449827720744, -4.613682088886104538, 70.79240656858107172 ) ) ;
#18502 = LINE ( 'NONE', #20432, #25405 ) ;
#18503 = CARTESIAN_POINT ( 'NONE',  ( 43.81606138205700063, -38.37466412126273951, 70.68129701848354784 ) ) ;
#18504 = VECTOR ( 'NONE', #12728, 1000.000000000000000 ) ;
#18505 = CARTESIAN_POINT ( 'NONE',  ( 31.81606138205700418, -36.10876147765401356, 70.30501292737011454 ) ) ;
#18506 = VECTOR ( 'NONE', #25161, 1000.000000000000000 ) ;
#18507 = DIRECTION ( 'NONE',  ( 0.000000000000000000, -1.000000000000000000, 3.469446951953613400E-15 ) ) ;
#18508 = CARTESIAN_POINT ( 'NONE',  ( 37.80737592653075296, -5.262488812442727593, 82.80487014872778673 ) ) ;
#18509 = VECTOR ( 'NONE', #11760, 1000.000000000000000 ) ;
#18510 = PLANE ( 'NONE',  #5798 ) ;
#18511 = VERTEX_POINT ( 'NONE', #7444 ) ;
#18512 = ORIENTED_EDGE ( 'NONE', *, *, #25086, .F. ) ;
#18513 = DIRECTION ( 'NONE',  ( 1.000000000000000000, 0.000000000000000000, 0.000000000000000000 ) ) ;
#18514 = CARTESIAN_POINT ( 'NONE',  ( 38.37017380507020192, -28.01368208888610667, 73.71602215082113219 ) ) ;
#18515 = CARTESIAN_POINT ( 'NONE',  ( 37.12184278917507640, -19.51368208888610312, 71.43714994484034264 ) ) ;
#18516 = ORIENTED_EDGE ( 'NONE', *, *, #19863, .F. ) ;
#18517 = ORIENTED_EDGE ( 'NONE', *, *, #20605, .T. ) ;
#18518 = CARTESIAN_POINT ( 'NONE',  ( 36.31606138205700063, -29.06829118875199924, 75.30501292737000085 ) ) ;
#18519 = CARTESIAN_POINT ( 'NONE',  ( 39.98359781491296161, -2.413682088886103472, 71.86517103874048473 ) ) ;
#18520 = CARTESIAN_POINT ( 'NONE',  ( 38.37017380507018771, -1.603840866421912148, 70.24448340153877268 ) ) ;
#18521 = VECTOR ( 'NONE', #24348, 1000.000000000000227 ) ;
#18522 = DIRECTION ( 'NONE',  ( -1.000000000000000000, -1.734723475976804876E-16, 1.734723475976814737E-16 ) ) ;
#18523 = CARTESIAN_POINT ( 'NONE',  ( 40.55423172469004811, -6.413682088886103472, 72.05058123536544201 ) ) ;
#18524 = VECTOR ( 'NONE', #8696, 1000.000000000000000 ) ;
#18525 = DIRECTION ( 'NONE',  ( 0.000000000000000000, 0.7540134720837676774, 0.6568589528324791926 ) ) ;
#18526 = DIRECTION ( 'NONE',  ( -1.000000000000000000, 5.204170427930415223E-30, 1.734723475976805122E-15 ) ) ;
#18527 = CARTESIAN_POINT ( 'NONE',  ( 33.77220352641053580, 2.787451151481231015, 6.090842338480662477 ) ) ;
#18528 = CARTESIAN_POINT ( 'NONE',  ( 44.81606138205700063, -34.55876147765410167, 66.30501292737000085 ) ) ;
#18529 = EDGE_CURVE ( 'NONE', #17733, #9987, #21478, .T. ) ;
#18530 = CARTESIAN_POINT ( 'NONE',  ( 40.25357836725066818, -6.620057786443027226, 82.69997634557660149 ) ) ;
#18531 = LINE ( 'NONE', #385, #10208 ) ;
#18532 = EDGE_CURVE ( 'NONE', #9258, #11322, #6067, .T. ) ;
#18533 = EDGE_CURVE ( 'NONE', #20770, #15469, #2354, .T. ) ;
#18534 = CARTESIAN_POINT ( 'NONE',  ( 44.81606138205700063, -26.74044063519535186, 84.30501292737007191 ) ) ;
#18535 = EDGE_CURVE ( 'NONE', #17183, #11291, #3591, .T. ) ;
#18536 = ORIENTED_EDGE ( 'NONE', *, *, #5951, .T. ) ;
#18537 = CARTESIAN_POINT ( 'NONE',  ( 39.90994555940143584, -21.43601452184545764, 75.33022986137839894 ) ) ;
#18538 = CARTESIAN_POINT ( 'NONE',  ( 33.56606138205700773, 41.44123852234599070, 73.55501292736987295 ) ) ;
#18539 = EDGE_LOOP ( 'NONE', ( #13590, #8529, #16995, #19681, #23938 ) ) ;
#18540 = ORIENTED_EDGE ( 'NONE', *, *, #21868, .T. ) ;
#18541 = UNCERTAINTY_MEASURE_WITH_UNIT (LENGTH_MEASURE( 1.000000000000000082E-05 ), #13905, 'distance_accuracy_value', 'NONE');
#18542 = VECTOR ( 'NONE', #16596, 1000.000000000000000 ) ;
#18543 = CARTESIAN_POINT ( 'NONE',  ( 36.07789103942399578, -20.20384086642191335, 72.05058123536544201 ) ) ;
#18544 = ADVANCED_FACE ( 'NONE', ( #5763 ), #3826, .F. ) ;
#18545 = CARTESIAN_POINT ( 'NONE',  ( 37.80618814713140097, -19.91368208888610170, 73.13360434286903455 ) ) ;
#18546 = DIRECTION ( 'NONE',  ( 1.000000000000000000, -5.204170427930413997E-31, -1.734723475976804876E-16 ) ) ;
#18547 = EDGE_CURVE ( 'NONE', #18363, #10132, #15678, .T. ) ;
#18548 = PLANE ( 'NONE',  #20074 ) ;
#18549 =( NAMED_UNIT ( * ) SI_UNIT ( $, .STERADIAN. ) SOLID_ANGLE_UNIT ( ) );
#18550 = VERTEX_POINT ( 'NONE', #12085 ) ;
#18551 = FACE_OUTER_BOUND ( 'NONE', #8178, .T. ) ;
#18552 = CARTESIAN_POINT ( 'NONE',  ( 43.31606138205700063, 7.535758204303438568, 66.26723409915207696 ) ) ;
#18553 = CARTESIAN_POINT ( 'NONE',  ( 40.55423172469004101, 0.7961591335780838774, 70.70992431699450265 ) ) ;
#18554 = VERTEX_POINT ( 'NONE', #15808 ) ;
#18555 = DIRECTION ( 'NONE',  ( 0.000000000000000000, 1.000000000000000000, -2.999999999999999839E-15 ) ) ;
#18556 = DIRECTION ( 'NONE',  ( 0.000000000000000000, -0.9992330079037401447, 0.03915859951075795903 ) ) ;
#18557 = CARTESIAN_POINT ( 'NONE',  ( 39.38009889167650357, -2.213682088886108179, 72.75271321436733274 ) ) ;
#18558 = CARTESIAN_POINT ( 'NONE',  ( 30.81606138205700418, 40.39281886181299797, 82.55501292736983032 ) ) ;
#18559 = CARTESIAN_POINT ( 'NONE',  ( 36.80608444377001121, -21.31368208888610027, 70.35351908239860563 ) ) ;
#18560 = AXIS2_PLACEMENT_3D ( 'NONE', #20956, #24668, #20701 ) ;
#18561 = CARTESIAN_POINT ( 'NONE',  ( 38.96215273200666473, -22.12375471166958008, 75.80539210339577494 ) ) ;
#18562 = CARTESIAN_POINT ( 'NONE',  ( 30.81606138205697931, 1.361611432489137741, -2.592146606185725677 ) ) ;
#18563 = CARTESIAN_POINT ( 'NONE',  ( 37.38336156205273397, -17.90384086642190908, 70.63227792289247020 ) ) ;
#18564 = CARTESIAN_POINT ( 'NONE',  ( 38.82593461698262871, -6.913682088886100807, 69.62690120949091011 ) ) ;
#18565 = ORIENTED_EDGE ( 'NONE', *, *, #13651, .F. ) ;
#18566 = CARTESIAN_POINT ( 'NONE',  ( 36.06606138205694378, 4.312150376739267266, 4.986822452676363149 ) ) ;
#18567 = VERTEX_POINT ( 'NONE', #13758 ) ;
#18568 = CARTESIAN_POINT ( 'NONE',  ( 39.38009889167648936, -7.403840866421908196, 70.00779233799264034 ) ) ;
#18569 = CARTESIAN_POINT ( 'NONE',  ( 33.31606138205700773, -4.357181138186127178, 82.80501292736992980 ) ) ;
#18570 = CARTESIAN_POINT ( 'NONE',  ( 38.93415946300897446, -4.113682088886107202, 73.09843995877331224 ) ) ;
#18571 = ORIENTED_EDGE ( 'NONE', *, *, #16885, .F. ) ;
#18572 = CARTESIAN_POINT ( 'NONE',  ( 36.98690846071097837, -9.813682088886107380, 73.30173637941818754 ) ) ;
#18573 = ORIENTED_EDGE ( 'NONE', *, *, #20567, .F. ) ;
#18574 = DIRECTION ( 'NONE',  ( 0.000000000000000000, -0.9911113317706403691, -0.1330350631819583740 ) ) ;
#18575 = CARTESIAN_POINT ( 'NONE',  ( 37.69225076346193504, -11.80384086642191477, 70.42958956619168021 ) ) ;
#18576 = ORIENTED_EDGE ( 'NONE', *, *, #9414, .T. ) ;
#18577 = ORIENTED_EDGE ( 'NONE', *, *, #8964, .F. ) ;
#18578 = FACE_OUTER_BOUND ( 'NONE', #1339, .T. ) ;
#18579 = LINE ( 'NONE', #8806, #5091 ) ;
#18580 = CARTESIAN_POINT ( 'NONE',  ( 38.26194895904384197, -14.60384086642191726, 73.71602215082113219 ) ) ;
#18581 = CARTESIAN_POINT ( 'NONE',  ( 37.79585267494195477, -22.16019180447545622, 75.81017787406068464 ) ) ;
#18582 = DIRECTION ( 'NONE',  ( 1.000000000000000000, 0.000000000000000000, 0.000000000000000000 ) ) ;
#18583 = CARTESIAN_POINT ( 'NONE',  ( 39.82603832034400426, -20.31368208888610738, 72.40698646996133903 ) ) ;
#18584 = DIRECTION ( 'NONE',  ( -1.734723475976807292E-15, 0.7516416929448820339, 0.6595716529892350355 ) ) ;
#18585 = ADVANCED_FACE ( 'NONE', ( #17748 ), #6021, .T. ) ;
#18586 = CARTESIAN_POINT ( 'NONE',  ( 44.81606138205700063, -38.55876147765349771, 84.30501292737325514 ) ) ;
#18587 = EDGE_LOOP ( 'NONE', ( #13828, #9937, #25142, #7622 ) ) ;
#18588 = DIRECTION ( 'NONE',  ( 0.000000000000000000, 0.8212051873014223347, 0.5706330172266899092 ) ) ;
#18589 = CARTESIAN_POINT ( 'NONE',  ( 32.56606138205700773, 40.39281886181299797, 82.55501292736983032 ) ) ;
#18590 = AXIS2_PLACEMENT_3D ( 'NONE', #1250, #12741, #6667 ) ;
#18591 = CARTESIAN_POINT ( 'NONE',  ( 37.69796330110505522, -12.50384086642191406, 73.09843995877329803 ) ) ;
#18592 = LINE ( 'NONE', #8937, #5084 ) ;
#18593 = DIRECTION ( 'NONE',  ( -1.734723475976804876E-16, -3.491481338843135327E-15, -1.000000000000000000 ) ) ;
#18594 = CARTESIAN_POINT ( 'NONE',  ( 40.31606138205700773, -21.45740613484709769, 28.95788407061096237 ) ) ;
#18595 = CARTESIAN_POINT ( 'NONE',  ( 36.68196826583682935, -26.00384086642191406, 70.79240656858105751 ) ) ;
#18596 = CARTESIAN_POINT ( 'NONE',  ( 36.31606138205700063, -6.858712374802629519, 82.66539206659815875 ) ) ;
#18597 = VERTEX_POINT ( 'NONE', #10269 ) ;
#18598 = CARTESIAN_POINT ( 'NONE',  ( 36.80608444377001121, -23.31368208888610383, 70.35351908239857721 ) ) ;
#18599 = EDGE_LOOP ( 'NONE', ( #5346, #23030, #15879, #15656 ) ) ;
#18600 = EDGE_LOOP ( 'NONE', ( #9049, #10302, #2763, #24399 ) ) ;
#18601 = CARTESIAN_POINT ( 'NONE',  ( 42.81606138205700063, 16.19123852234701388, 73.80501292736995822 ) ) ;
#18602 = LINE ( 'NONE', #18483, #10877 ) ;
#18603 = CARTESIAN_POINT ( 'NONE',  ( 38.37017380507020192, -0.01368208888610084051, 72.51602215082118619 ) ) ;
#18604 = CARTESIAN_POINT ( 'NONE',  ( 38.73920764526923932, -29.50384086642191050, 70.26206559358661252 ) ) ;
#18605 = ORIENTED_EDGE ( 'NONE', *, *, #20753, .T. ) ;
#18606 = ORIENTED_EDGE ( 'NONE', *, *, #7665, .F. ) ;
#18607 = CARTESIAN_POINT ( 'NONE',  ( 35.31606138205687273, 43.19123852234595518, 61.80501292736988006 ) ) ;
#18608 = CARTESIAN_POINT ( 'NONE',  ( 36.31606138205700063, -11.51539968388052060, 18.41550321377400934 ) ) ;
#18609 = ORIENTED_EDGE ( 'NONE', *, *, #9283, .F. ) ;
#18610 = DIRECTION ( 'NONE',  ( -1.327674326049719602E-15, 0.4425581086832399147, -0.8967398287344627850 ) ) ;
#18611 = CARTESIAN_POINT ( 'NONE',  ( 39.75915168707251723, -6.903840866421915301, 72.49904802271740323 ) ) ;
#18612 = VECTOR ( 'NONE', #11193, 1000.000000000000227 ) ;
#18613 = EDGE_CURVE ( 'NONE', #22481, #170, #2138, .T. ) ;
#18614 = EDGE_CURVE ( 'NONE', #2590, #7328, #21611, .T. ) ;
#18615 = CYLINDRICAL_SURFACE ( 'NONE', #18284, 1.100000000000000311 ) ;
#18616 = EDGE_CURVE ( 'NONE', #6360, #10501, #8209, .T. ) ;
#18617 = DIRECTION ( 'NONE',  ( -4.298950768721509852E-32, 1.000000000000000000, -3.115648231731786715E-15 ) ) ;
#18618 = ORIENTED_EDGE ( 'NONE', *, *, #24176, .T. ) ;
#18619 = ORIENTED_EDGE ( 'NONE', *, *, #15799, .F. ) ;
#18620 = ORIENTED_EDGE ( 'NONE', *, *, #18660, .F. ) ;
#18621 = CARTESIAN_POINT ( 'NONE',  ( 44.81606138205700063, 41.44123852234599781, 75.30501292736987295 ) ) ;
#18622 = CARTESIAN_POINT ( 'NONE',  ( 36.80608444377001121, -1.313682088886099830, 70.35351908239861984 ) ) ;
#18623 = CIRCLE ( 'NONE', #19438, 1.750000000000001554 ) ;
#18624 = CARTESIAN_POINT ( 'NONE',  ( 39.89531854050225235, -29.10876147765329591, 71.21617469530100664 ) ) ;
#18625 = DIRECTION ( 'NONE',  ( 1.734723475976805122E-15, 2.999999999999999839E-15, 1.000000000000000000 ) ) ;
#18626 = ORIENTED_EDGE ( 'NONE', *, *, #10385, .T. ) ;
#18627 = FACE_OUTER_BOUND ( 'NONE', #23521, .T. ) ;
#18628 = ADVANCED_FACE ( 'NONE', ( #21989 ), #11964, .T. ) ;
#18629 = VECTOR ( 'NONE', #4561, 1000.000000000000114 ) ;
#18630 = VECTOR ( 'NONE', #1976, 1000.000000000000000 ) ;
#18631 = CYLINDRICAL_SURFACE ( 'NONE', #9050, 1.000000000000012657 ) ;
#18632 = DIRECTION ( 'NONE',  ( 0.000000000000000000, 0.5706330172266920187, -0.8212051873014210024 ) ) ;
#18633 = SURFACE_SIDE_STYLE ('',( #18762 ) ) ;
#18634 = CIRCLE ( 'NONE', #5471, 3.000000000000002665 ) ;
#18635 = CARTESIAN_POINT ( 'NONE',  ( 30.81606138205698642, -8.004447042669500689, -3.950346388939002029 ) ) ;
#18636 = VERTEX_POINT ( 'NONE', #16056 ) ;
#18637 = ORIENTED_EDGE ( 'NONE', *, *, #19820, .F. ) ;
#18638 = FACE_OUTER_BOUND ( 'NONE', #15824, .T. ) ;
#18639 = DIRECTION ( 'NONE',  ( 0.000000000000000000, 0.5706330172266919076, -0.8212051873014208914 ) ) ;
#18640 = CARTESIAN_POINT ( 'NONE',  ( 37.31647492878122563, -19.31368208888610027, 70.72433947564853440 ) ) ;
#18641 = ORIENTED_EDGE ( 'NONE', *, *, #18397, .T. ) ;
#18642 = CIRCLE ( 'NONE', #10012, 1.000000000000000888 ) ;
#18643 = ORIENTED_EDGE ( 'NONE', *, *, #9929, .T. ) ;
#18644 = DIRECTION ( 'NONE',  ( 0.000000000000000000, 1.000000000000000000, 0.000000000000000000 ) ) ;
#18645 = CARTESIAN_POINT ( 'NONE',  ( 37.80618814713140097, 0.08631791111389161553, 73.13360434286904876 ) ) ;
#18646 = CARTESIAN_POINT ( 'NONE',  ( 39.95015449827720744, -23.00384086642191050, 71.96809898377887293 ) ) ;
#18647 = DIRECTION ( 'NONE',  ( 1.000000000000000000, 0.000000000000000000, 0.000000000000000000 ) ) ;
#18648 = B_SPLINE_CURVE_WITH_KNOTS ( 'NONE', 3,
 ( #6550, #12500, #18157, #8495, #14538, #8108, #10165, #21889, #4249, #18409 ),
 .UNSPECIFIED., .F., .F.,
 ( 4, 3, 3, 4 ),
 ( 2.436441354035134762E-18, 0.0001278088409237286072, 0.0002582060142820110401, 0.0003905966221991465331 ),
 .UNSPECIFIED. ) ;
#18649 = CIRCLE ( 'NONE', #10019, 0.7500000000000006661 ) ;
#18650 = CARTESIAN_POINT ( 'NONE',  ( 35.86008812008917346, -11.51368208888610134, 71.43714994484034264 ) ) ;
#18651 = CIRCLE ( 'NONE', #23986, 1.250000000000000888 ) ;
#18652 = DIRECTION ( 'NONE',  ( -1.225631768639319301E-15, 0.4425581086832399147, -0.8967398287344627850 ) ) ;
#18653 = LINE ( 'NONE', #18780, #6680 ) ;
#18654 = VECTOR ( 'NONE', #10316, 1000.000000000000227 ) ;
#18655 = FACE_BOUND ( 'NONE', #18372, .T. ) ;
#18656 = PLANE ( 'NONE',  #4221 ) ;
#18657 = CARTESIAN_POINT ( 'NONE',  ( 38.14273442609844977, 38.69123852234599781, 70.32014858831708182 ) ) ;
#18658 = VECTOR ( 'NONE', #20941, 1000.000000000000000 ) ;
#18659 = DIRECTION ( 'NONE',  ( 0.000000000000000000, 2.999999999999999839E-15, 1.000000000000000000 ) ) ;
#18660 = EDGE_CURVE ( 'NONE', #10892, #10558, #11832, .T. ) ;
#18661 = DIRECTION ( 'NONE',  ( 1.000000000000000000, 0.000000000000000000, 0.000000000000000000 ) ) ;
#18662 = ORIENTED_EDGE ( 'NONE', *, *, #16079, .F. ) ;
#18663 = CARTESIAN_POINT ( 'NONE',  ( 44.81606138205700063, 35.44123852234597649, 67.80501292736990138 ) ) ;
#18664 = DIRECTION ( 'NONE',  ( -4.625929269271484533E-15, 0.8967398287344634511, 0.4425581086832385824 ) ) ;
#18665 = ORIENTED_EDGE ( 'NONE', *, *, #12929, .F. ) ;
#18666 = EDGE_LOOP ( 'NONE', ( #5195, #6641, #23977, #24220 ) ) ;
#18667 = VECTOR ( 'NONE', #4375, 1000.000000000000000 ) ;
#18668 = CARTESIAN_POINT ( 'NONE',  ( 40.26954217208372455, -14.90384086642191797, 72.86986841596734621 ) ) ;
#18669 = AXIS2_PLACEMENT_3D ( 'NONE', #22795, #3204, #1278 ) ;
#18670 = CARTESIAN_POINT ( 'NONE',  ( 38.82593461698262871, -20.91368208888609459, 69.62690120949091011 ) ) ;
#18671 = LINE ( 'NONE', #1010, #13221 ) ;
#18672 = EDGE_CURVE ( 'NONE', #18480, #9092, #2014, .T. ) ;
#18673 = DIRECTION ( 'NONE',  ( 0.000000000000000000, -1.000000000000000000, 2.999999999999999839E-15 ) ) ;
#18675 = EDGE_CURVE ( 'NONE', #3732, #11745, #20054, .T. ) ;
#18674 =( LENGTH_UNIT ( ) NAMED_UNIT ( * ) SI_UNIT ( .MILLI., .METRE. ) );
#18676 = ORIENTED_EDGE ( 'NONE', *, *, #24453, .F. ) ;
#18677 = DIRECTION ( 'NONE',  ( 1.000000000000000000, 1.185941393278724777E-16, 8.240782279085522416E-17 ) ) ;
#18678 = CARTESIAN_POINT ( 'NONE',  ( 40.31606138205701484, -19.34822312381089660, 24.15308711316412627 ) ) ;
#18679 = CARTESIAN_POINT ( 'NONE',  ( 36.98690846071097837, -25.81368208888611093, 73.30173637941817333 ) ) ;
#18680 = ORIENTED_EDGE ( 'NONE', *, *, #16350, .F. ) ;
#18681 = EDGE_CURVE ( 'NONE', #17958, #10709, #4091, .T. ) ;
#18682 = CARTESIAN_POINT ( 'NONE',  ( 38.31606138205700063, 40.69123852234599781, 71.30501292737000085 ) ) ;
#18683 = LINE ( 'NONE', #8903, #14899 ) ;
#18684 = CARTESIAN_POINT ( 'NONE',  ( 36.64852494920107517, -3.413682088886104360, 70.89533451361948835 ) ) ;
#18685 = CARTESIAN_POINT ( 'NONE',  ( 32.81606138205700773, 35.95440708241085304, 62.30501292736990138 ) ) ;
#18686 = CARTESIAN_POINT ( 'NONE',  ( 38.82593461698262871, -22.91368208888609814, 69.62690120949091011 ) ) ;
#18687 = VECTOR ( 'NONE', #16954, 1000.000000000000000 ) ;
#18688 = DIRECTION ( 'NONE',  ( 1.512281363675413133E-17, 0.4425581086832396371, -0.8967398287344630070 ) ) ;
#18689 = VECTOR ( 'NONE', #14466, 1000.000000000000000 ) ;
#18690 = EDGE_CURVE ( 'NONE', #17085, #4130, #20182, .T. ) ;
#18691 = CARTESIAN_POINT ( 'NONE',  ( 33.31606138205700773, -21.26162886970023536, 44.16441745890789150 ) ) ;
#18692 = CARTESIAN_POINT ( 'NONE',  ( 38.63098279924290068, -20.70384086642191335, 72.53360434286904024 ) ) ;
#18693 = CARTESIAN_POINT ( 'NONE',  ( 39.95015449827720744, -6.613682088886106314, 70.79240656858107172 ) ) ;
#18694 = VERTEX_POINT ( 'NONE', #18133 ) ;
#18695 = CARTESIAN_POINT ( 'NONE',  ( 42.96606138205694947, 3.409598742320834930, 3.426245460917042074 ) ) ;
#18696 = EDGE_LOOP ( 'NONE', ( #7983, #16532 ) ) ;
#18697 = CARTESIAN_POINT ( 'NONE',  ( 37.33957961208645315, -3.803840866421909439, 69.94417936956673998 ) ) ;
#18698 = LINE ( 'NONE', #22684, #12331 ) ;
#18699 =( GEOMETRIC_REPRESENTATION_CONTEXT ( 3 ) GLOBAL_UNCERTAINTY_ASSIGNED_CONTEXT ( ( #7208 ) ) GLOBAL_UNIT_ASSIGNED_CONTEXT ( ( #12435, #24371, #8559 ) ) REPRESENTATION_CONTEXT ( 'NONE', 'WORKASPACE' ) );
#18700 = CARTESIAN_POINT ( 'NONE',  ( 37.69796330110504101, -5.113682088886101873, 69.66206559358663242 ) ) ;
#18701 = ORIENTED_EDGE ( 'NONE', *, *, #8810, .T. ) ;
#18702 = CARTESIAN_POINT ( 'NONE',  ( 39.12911128074873801, -12.11368208888610987, 73.69843995877327814 ) ) ;
#18703 = EDGE_LOOP ( 'NONE', ( #1868, #19531 ) ) ;
#18704 = CARTESIAN_POINT ( 'NONE',  ( 32.56606138205700773, 43.35512946304240245, 83.12823623207320622 ) ) ;
#18705 = CARTESIAN_POINT ( 'NONE',  ( 39.31564783533279694, -13.30384086642190944, 70.72433947564853440 ) ) ;
#18706 = EDGE_CURVE ( 'NONE', #13535, #19200, #9896, .T. ) ;
#18707 = SPHERICAL_SURFACE ( 'NONE', #4431, 1.100000000000000089 ) ;
#18708 = EDGE_CURVE ( 'NONE', #1835, #18383, #15146, .T. ) ;
#18709 = ORIENTED_EDGE ( 'NONE', *, *, #18172, .T. ) ;
#18710 = DIRECTION ( 'NONE',  ( 1.000000000000000000, -6.018531076210080512E-31, -1.734723475976804876E-16 ) ) ;
#18711 = CARTESIAN_POINT ( 'NONE',  ( 32.81606138205700773, -24.55876147765401996, 67.80501292737008612 ) ) ;
#18712 = CARTESIAN_POINT ( 'NONE',  ( 38.37017380507018771, -15.60384086642191370, 69.04448340153878405 ) ) ;
#18713 = EDGE_CURVE ( 'NONE', #12829, #18144, #19932, .T. ) ;
#18714 = EDGE_CURVE ( 'NONE', #562, #9681, #6150, .T. ) ;
#18715 = EDGE_CURVE ( 'NONE', #22433, #24927, #21734, .T. ) ;
#18716 = CARTESIAN_POINT ( 'NONE',  ( 38.31606138205700063, -22.22127907754186893, 75.80501292736997243 ) ) ;
#18717 = DIRECTION ( 'NONE',  ( 0.000000000000000000, 2.775557561562888984E-15, 1.000000000000000000 ) ) ;
#18718 = CARTESIAN_POINT ( 'NONE',  ( 38.82593461698262871, -20.91368208888609459, 69.62690120949091011 ) ) ;
#18719 = PLANE ( 'NONE',  #21180 ) ;
#18720 = DIRECTION ( 'NONE',  ( -1.000000000000000000, 0.000000000000000000, 0.000000000000000000 ) ) ;
#18721 = ORIENTED_EDGE ( 'NONE', *, *, #18260, .F. ) ;
#18722 = PLANE ( 'NONE',  #9633 ) ;
#18723 = CARTESIAN_POINT ( 'NONE',  ( 33.31606138205700773, -27.60498114914039647, 57.04949906928990089 ) ) ;
#18724 = CARTESIAN_POINT ( 'NONE',  ( 36.87297107704151244, -15.90384086642190908, 70.26145752964255564 ) ) ;
#18725 = AXIS2_PLACEMENT_3D ( 'NONE', #7753, #15595, #10188 ) ;
#18726 = CARTESIAN_POINT ( 'NONE',  ( 0.000000000000000000, 0.000000000000000000, 0.000000000000000000 ) ) ;
#18727 = CYLINDRICAL_SURFACE ( 'NONE', #3423, 0.7500000000000006661 ) ;
#18728 = CARTESIAN_POINT ( 'NONE',  ( 39.95015449827720744, -24.61368208888610454, 70.79240656858104330 ) ) ;
#18729 = DIRECTION ( 'NONE',  ( -1.000000000000000000, 0.000000000000000000, 0.000000000000000000 ) ) ;
#18730 = CARTESIAN_POINT ( 'NONE',  ( 37.69796330110505522, -22.50384086642191050, 73.09843995877329803 ) ) ;
#18731 = CARTESIAN_POINT ( 'NONE',  ( 38.31606138205700063, -5.204193249396280585, 82.80501292736992980 ) ) ;
#18732 = EDGE_CURVE ( 'NONE', #23179, #3938, #14009, .T. ) ;
#18733 = CARTESIAN_POINT ( 'NONE',  ( 36.87297107704152666, -21.71368208888610951, 72.49904802271740323 ) ) ;
#18734 = ORIENTED_EDGE ( 'NONE', *, *, #17169, .T. ) ;
#18735 = ORIENTED_EDGE ( 'NONE', *, *, #1219, .T. ) ;
#18736 = CARTESIAN_POINT ( 'NONE',  ( 41.14099152588522657, 1.392818861812999964, 84.30501292737000085 ) ) ;
#18737 = FACE_BOUND ( 'NONE', #25463, .T. ) ;
#18738 = CARTESIAN_POINT ( 'NONE',  ( 39.31564783533279694, -29.30384086642190766, 70.72433947564850598 ) ) ;
#18739 = CARTESIAN_POINT ( 'NONE',  ( 38.73920764526925353, -0.1136820888861002354, 72.49843995877331793 ) ) ;
#18740 = ORIENTED_EDGE ( 'NONE', *, *, #5246, .T. ) ;
#18741 = VERTEX_POINT ( 'NONE', #22615 ) ;
#18742 = CARTESIAN_POINT ( 'NONE',  ( 37.31606138205702194, -21.82181003913286688, 31.95585308007612468 ) ) ;
#18743 = FACE_OUTER_BOUND ( 'NONE', #11866, .T. ) ;
#18744 = ORIENTED_EDGE ( 'NONE', *, *, #23926, .T. ) ;
#18745 = PLANE ( 'NONE',  #6114 ) ;
#18746 = CARTESIAN_POINT ( 'NONE',  ( 39.29254315202757653, -2.803840866421915212, 72.81632618279323310 ) ) ;
#18747 = VECTOR ( 'NONE', #7854, 1000.000000000000000 ) ;
#18748 = FACE_OUTER_BOUND ( 'NONE', #17826, .T. ) ;
#18749 = DIRECTION ( 'NONE',  ( 0.000000000000000000, 1.000000000000000000, 0.000000000000000000 ) ) ;
#18750 = ORIENTED_EDGE ( 'NONE', *, *, #20114, .T. ) ;
#18751 = ORIENTED_EDGE ( 'NONE', *, *, #17763, .T. ) ;
#18752 = ORIENTED_EDGE ( 'NONE', *, *, #796, .T. ) ;
#18753 = CARTESIAN_POINT ( 'NONE',  ( 45.81606138205707168, -37.70325315460877391, 65.37863370302704880 ) ) ;
#18754 = CARTESIAN_POINT ( 'NONE',  ( 37.80618814713140097, -1.913682088886106580, 73.13360434286904876 ) ) ;
#18755 = CARTESIAN_POINT ( 'NONE',  ( 40.02061183432068958, -29.10876147765278787, 71.40071884891759169 ) ) ;
#18756 = CARTESIAN_POINT ( 'NONE',  ( 29.71606138205695657, -23.19619402982949907, 47.16846523730000484 ) ) ;
#18757 = FACE_OUTER_BOUND ( 'NONE', #11976, .T. ) ;
#18758 = DIRECTION ( 'NONE',  ( 0.6648258951495188418, -0.6134389167572597001, -0.4262619201222657694 ) ) ;
#18759 = EDGE_CURVE ( 'NONE', #5707, #235, #22365, .T. ) ;
#18760 = DIRECTION ( 'NONE',  ( 3.469446951953570407E-15, -0.8967398287344626739, -0.4425581086832399702 ) ) ;
#18761 = CARTESIAN_POINT ( 'NONE',  ( 36.31606138205700063, -7.108955154158179468, 82.62193108360246185 ) ) ;
#18762 = SURFACE_STYLE_FILL_AREA ( #5491 ) ;
#18763 = EDGE_CURVE ( 'NONE', #7399, #5590, #24655, .T. ) ;
#18764 = CARTESIAN_POINT ( 'NONE',  ( 40.31606138205700063, 5.691238522346988127, 65.30501292736998664 ) ) ;
#18765 = ORIENTED_EDGE ( 'NONE', *, *, #2151, .T. ) ;
#18766 = ORIENTED_EDGE ( 'NONE', *, *, #6723, .T. ) ;
#18767 = PLANE ( 'NONE',  #6663 ) ;
#18768 = CARTESIAN_POINT ( 'NONE',  ( 44.81606138205700063, 40.39281886181299797, 81.75501292736983316 ) ) ;
#18769 = CARTESIAN_POINT ( 'NONE',  ( 37.12184278917507640, -17.51368208888609956, 71.43714994484034264 ) ) ;
#18770 = ORIENTED_EDGE ( 'NONE', *, *, #18390, .T. ) ;
#18771 = EDGE_LOOP ( 'NONE', ( #21327, #19816, #6227, #13916, #20051, #16197, #22632, #12038, #12128, #6539, #14016, #1896, #5783, #11203, #19276, #7911 ) ) ;
#18772 = CARTESIAN_POINT ( 'NONE',  ( 40.31606138205700773, -16.77230293220685198, 77.52306850662458260 ) ) ;
#18773 = CARTESIAN_POINT ( 'NONE',  ( 39.29254315202756231, -0.8136820888860994971, 69.94417936956673998 ) ) ;
#18774 = CARTESIAN_POINT ( 'NONE',  ( 37.80618814713138676, -25.70384086642190979, 69.62690120949091011 ) ) ;
#18775 = LINE ( 'NONE', #10676, #14071 ) ;
#18776 = EDGE_CURVE ( 'NONE', #22473, #7941, #14878, .T. ) ;
#18777 = CARTESIAN_POINT ( 'NONE',  ( 40.33642880535524000, -8.313682088886110932, 72.77780686321128201 ) ) ;
#18778 = CARTESIAN_POINT ( 'NONE',  ( 38.31606138205700063, 42.51966564709218233, 71.30501292737018559 ) ) ;
#18779 = EDGE_LOOP ( 'NONE', ( #22466, #3574 ) ) ;
#18780 = CARTESIAN_POINT ( 'NONE',  ( 43.81606138205700063, -27.17722769842920272, 59.42551550655435477 ) ) ;
#18781 = CYLINDRICAL_SURFACE ( 'NONE', #14303, 2.000000000000001776 ) ;
#18782 = DIRECTION ( 'NONE',  ( 0.000000000000000000, 0.5706330172266919076, -0.8212051873014208914 ) ) ;
#18783 = CARTESIAN_POINT ( 'NONE',  ( 40.05520938202761982, -6.160151306619628286, 82.75976152844953049 ) ) ;
#18784 = FACE_OUTER_BOUND ( 'NONE', #24014, .T. ) ;
#18785 = EDGE_CURVE ( 'NONE', #3732, #2891, #2516, .T. ) ;
#18786 = CYLINDRICAL_SURFACE ( 'NONE', #22584, 1.500000000000001332 ) ;
#18787 = EDGE_CURVE ( 'NONE', #25070, #14577, #18376, .T. ) ;
#18788 = ORIENTED_EDGE ( 'NONE', *, *, #22550, .F. ) ;
#18789 = LINE ( 'NONE', #5393, #16020 ) ;
#18790 = LINE ( 'NONE', #2805, #9911 ) ;
#18791 = ORIENTED_EDGE ( 'NONE', *, *, #17847, .F. ) ;
#18792 = EDGE_LOOP ( 'NONE', ( #24366, #4311, #22977, #17800 ) ) ;
#18793 = UNCERTAINTY_MEASURE_WITH_UNIT (LENGTH_MEASURE( 1.000000000000000082E-05 ), #11924, 'distance_accuracy_value', 'NONE');
#18794 = CARTESIAN_POINT ( 'NONE',  ( 36.36258059203030513, -19.90384086642191264, 69.89063713639259845 ) ) ;
#18795 = CARTESIAN_POINT ( 'NONE',  ( 36.68196826583682935, -21.61368208888610454, 71.96809898377888715 ) ) ;
#18796 = DIRECTION ( 'NONE',  ( 0.000000000000000000, 1.000000000000000000, -2.999999999999999839E-15 ) ) ;
#18797 = DIRECTION ( 'NONE',  ( 0.000000000000000000, -1.000000000000000000, 2.775557561562890957E-15 ) ) ;
#18798 = EDGE_LOOP ( 'NONE', ( #9712, #5890, #17322, #18143 ) ) ;
#18799 = CARTESIAN_POINT ( 'NONE',  ( 45.81606138205706458, -35.90867894478441968, 74.07034463014319670 ) ) ;
#18800 = LINE ( 'NONE', #4890, #10459 ) ;
#18801 = EDGE_CURVE ( 'NONE', #21877, #2631, #4466, .T. ) ;
#18802 = CARTESIAN_POINT ( 'NONE',  ( 40.77203464402485622, 0.8961591335780867418, 71.43714994484035685 ) ) ;
#18803 = VECTOR ( 'NONE', #21541, 1000.000000000000000 ) ;
#18804 = ORIENTED_EDGE ( 'NONE', *, *, #23166, .T. ) ;
#18805 = DIRECTION ( 'NONE',  ( -1.000000000000000000, 0.000000000000000000, 0.000000000000000000 ) ) ;
#18806 = CARTESIAN_POINT ( 'NONE',  ( 32.81606138205700773, -34.55876147765400930, 73.55501292737011454 ) ) ;
#18807 = AXIS2_PLACEMENT_3D ( 'NONE', #2236, #17970, #294 ) ;
#18808 = VECTOR ( 'NONE', #4159, 1000.000000000000000 ) ;
#18809 = CARTESIAN_POINT ( 'NONE',  ( 38.37017380507020192, -0.01368208888610777940, 73.11602215082118050 ) ) ;
#18810 = CARTESIAN_POINT ( 'NONE',  ( 31.81606138205700418, 40.34464305740947054, 81.44836866983821722 ) ) ;
#18811 = CARTESIAN_POINT ( 'NONE',  ( 36.87297107704153376, -21.71368208888610951, 72.49904802271740323 ) ) ;
#18812 = LINE ( 'NONE', #6833, #13177 ) ;
#18813 = CARTESIAN_POINT ( 'NONE',  ( 33.66606138205698073, -6.570990706613086374, -2.335727660491067503 ) ) ;
#18814 = CARTESIAN_POINT ( 'NONE',  ( 37.31647492878124694, -16.30384086642191122, 72.03616607671141026 ) ) ;
#18815 = CARTESIAN_POINT ( 'NONE',  ( 37.69796330110504101, -3.113682088886098764, 69.66206559358663242 ) ) ;
#18816 = CYLINDRICAL_SURFACE ( 'NONE', #10265, 1.550000000000002709 ) ;
#18817 = ORIENTED_EDGE ( 'NONE', *, *, #2787, .F. ) ;
#18818 = CLOSED_SHELL ( 'NONE', ( #9135, #25236, #7395, #17629 ) ) ;
#18819 = CARTESIAN_POINT ( 'NONE',  ( 37.80618814713138676, -5.703840866421908018, 69.62690120949091011 ) ) ;
#18820 = DIRECTION ( 'NONE',  ( -1.327674326049709741E-15, 0.4425581086832367506, -0.8967398287344643393 ) ) ;
#18821 = AXIS2_PLACEMENT_3D ( 'NONE', #18062, #2073, #18318 ) ;
#18822 = VECTOR ( 'NONE', #19779, 1000.000000000000000 ) ;
#18823 = CARTESIAN_POINT ( 'NONE',  ( 38.93415946300897446, -8.113682088886108090, 73.09843995877331224 ) ) ;
#18824 = ORIENTED_EDGE ( 'NONE', *, *, #23041, .F. ) ;
#18825 = CARTESIAN_POINT ( 'NONE',  ( 38.26194895904383486, -7.013682088886100452, 69.04448340153881247 ) ) ;
#18826 = ORIENTED_EDGE ( 'NONE', *, *, #509, .F. ) ;
#18827 = LINE ( 'NONE', #22939, #18131 ) ;
#18828 = CARTESIAN_POINT ( 'NONE',  ( 38.63098279924290068, -12.70384086642191157, 72.53360434286904024 ) ) ;
#18829 = ORIENTED_EDGE ( 'NONE', *, *, #594, .T. ) ;
#18830 = EDGE_LOOP ( 'NONE', ( #11657, #8443, #12167, #13745 ) ) ;
#18831 = PLANE ( 'NONE',  #11736 ) ;
#18832 = DIRECTION ( 'NONE',  ( 0.000000000000000000, 0.8212051873014223347, 0.5706330172266899092 ) ) ;
#18833 = ADVANCED_FACE ( 'NONE', ( #706 ), #22236, .T. ) ;
#18834 = CARTESIAN_POINT ( 'NONE',  ( 36.89935272106205133, -18.40384086642191974, 73.23812341099225875 ) ) ;
#18835 = CARTESIAN_POINT ( 'NONE',  ( 36.41626118072728246, -20.85991497674728024, 75.39736199887265400 ) ) ;
#18836 = CARTESIAN_POINT ( 'NONE',  ( 32.81606138205700773, 6.294683054830111146, 7.131205101789720224 ) ) ;
#18837 = CARTESIAN_POINT ( 'NONE',  ( 36.64852494920107517, -19.41368208888610525, 70.89533451361947414 ) ) ;
#18838 = PLANE ( 'NONE',  #22097 ) ;
#18839 = DIRECTION ( 'NONE',  ( 0.000000000000000000, -1.000000000000000000, 2.999999999999999839E-15 ) ) ;
#18840 = VECTOR ( 'NONE', #5017, 1000.000000000000000 ) ;
#18841 = ORIENTED_EDGE ( 'NONE', *, *, #2924, .T. ) ;
#18842 = VECTOR ( 'NONE', #6106, 1000.000000000000000 ) ;
#18843 = CIRCLE ( 'NONE', #16364, 1.000000000000000888 ) ;
#18844 = DIRECTION ( 'NONE',  ( 1.000000000000000000, 0.000000000000000000, 0.000000000000000000 ) ) ;
#18845 = DIRECTION ( 'NONE',  ( 1.000000000000000000, -3.982629455510873500E-31, -4.336808689942015271E-16 ) ) ;
#18846 = CARTESIAN_POINT ( 'NONE',  ( 37.69796330110505522, -6.503840866421914058, 73.09843995877331224 ) ) ;
#18847 = CARTESIAN_POINT ( 'NONE',  ( 0.000000000000000000, 0.000000000000000000, 0.000000000000000000 ) ) ;
#18848 = DIRECTION ( 'NONE',  ( -1.000000000000000000, -1.187136597504755470E-16, -8.249087426255173666E-17 ) ) ;
#18849 = EDGE_CURVE ( 'NONE', #11199, #17700, #16429, .T. ) ;
#18850 = CARTESIAN_POINT ( 'NONE',  ( 40.14115730948191185, -22.51368208888609956, 71.32335560751960202 ) ) ;
#18851 = EDGE_CURVE ( 'NONE', #5857, #6034, #6647, .T. ) ;
#18852 = DIRECTION ( 'NONE',  ( 1.000000000000000000, 2.104045878896135585E-30, -1.734723475976805122E-15 ) ) ;
#18853 = EDGE_CURVE ( 'NONE', #18511, #21676, #12596, .T. ) ;
#18854 = ADVANCED_FACE ( 'NONE', ( #12716 ), #2892, .T. ) ;
#18855 = CARTESIAN_POINT ( 'NONE',  ( 36.68196826583682935, -24.00384086642191050, 70.79240656858105751 ) ) ;
#18856 = EDGE_CURVE ( 'NONE', #16162, #18363, #18502, .T. ) ;
#18857 = DIRECTION ( 'NONE',  ( -0.9835979625596985576, -0.1803747433772529551, 0.000000000000000000 ) ) ;
#18858 = CARTESIAN_POINT ( 'NONE',  ( 37.69796330110504101, -27.11368208888609388, 69.66206559358660400 ) ) ;
#18859 = EDGE_LOOP ( 'NONE', ( #14874, #22019, #19012, #11755 ) ) ;
#18860 = ORIENTED_EDGE ( 'NONE', *, *, #2586, .F. ) ;
#18861 = DIRECTION ( 'NONE',  ( 1.000000000000000000, 2.740734061208483951E-15, -1.279526567694519919E-16 ) ) ;
#18862 = CARTESIAN_POINT ( 'NONE',  ( 29.81606138205697931, -5.918777154956199382, -5.916875169744970187 ) ) ;
#18863 = CARTESIAN_POINT ( 'NONE',  ( 39.02742774030102879, -0.2136820888860996304, 72.26730301774236409 ) ) ;
#18864 = VECTOR ( 'NONE', #14881, 1000.000000000000000 ) ;
#18865 = VERTEX_POINT ( 'NONE', #14758 ) ;
#18866 = ORIENTED_EDGE ( 'NONE', *, *, #3752, .T. ) ;
#18867 = CARTESIAN_POINT ( 'NONE',  ( 34.81606138205696510, -1.975699482566735776, -4.057200616784870206 ) ) ;
#18868 = CARTESIAN_POINT ( 'NONE',  ( 43.78068403493972482, 3.723062046805433845, 6.249772126726830912 ) ) ;
#18869 = ORIENTED_EDGE ( 'NONE', *, *, #10136, .T. ) ;
#18870 = EDGE_CURVE ( 'NONE', #15010, #15653, #17625, .T. ) ;
#18871 = PLANE ( 'NONE',  #12415 ) ;
#18872 = CARTESIAN_POINT ( 'NONE',  ( 39.75915168707251723, -2.903840866421913525, 72.49904802271740323 ) ) ;
#18873 = EDGE_CURVE ( 'NONE', #4444, #20177, #8724, .T. ) ;
#18874 = VECTOR ( 'NONE', #5788, 1000.000000000000227 ) ;
#18875 = DIRECTION ( 'NONE',  ( 0.000000000000000000, 1.000000000000000000, -2.999999999999999839E-15 ) ) ;
#18876 = DIRECTION ( 'NONE',  ( 1.271715504244016160E-15, -0.4425581086832399147, 0.8967398287344627850 ) ) ;
#18877 = ORIENTED_EDGE ( 'NONE', *, *, #3899, .T. ) ;
#18878 = ORIENTED_EDGE ( 'NONE', *, *, #15213, .F. ) ;
#18879 = ORIENTED_EDGE ( 'NONE', *, *, #1421, .T. ) ;
#18880 = LINE ( 'NONE', #4722, #7134 ) ;
#18881 = CARTESIAN_POINT ( 'NONE',  ( 38.93415946300898867, -0.1136820888861071605, 73.09843995877331224 ) ) ;
#18882 = ADVANCED_FACE ( 'NONE', ( #1088 ), #8975, .T. ) ;
#18883 = CARTESIAN_POINT ( 'NONE',  ( 40.14115730948191185, -25.10384086642190837, 71.43714994484030001 ) ) ;
#18884 = FILL_AREA_STYLE_COLOUR ( '', #19093 ) ;
#18885 = DIRECTION ( 'NONE',  ( -7.570943305532639295E-31, -1.000000000000000000, -4.914813388431354887E-16 ) ) ;
#18886 = VECTOR ( 'NONE', #16525, 1000.000000000000227 ) ;
#18887 = ORIENTED_EDGE ( 'NONE', *, *, #12095, .T. ) ;
#18888 = CARTESIAN_POINT ( 'NONE',  ( 41.81606138205687273, 43.19123852234595518, 61.80501292736988006 ) ) ;
#18889 = DIRECTION ( 'NONE',  ( 0.000000000000000000, -1.000000000000000000, 2.775557561562890957E-15 ) ) ;
#18890 = FACE_OUTER_BOUND ( 'NONE', #13358, .T. ) ;
#18891 = CARTESIAN_POINT ( 'NONE',  ( 36.31606138205700063, 5.691238522346989903, 65.80501292736998664 ) ) ;
#18892 = CIRCLE ( 'NONE', #7788, 1.750000000000001554 ) ;
#18893 = DIRECTION ( 'NONE',  ( 1.156482317317872465E-16, 0.4425581086832399702, -0.8967398287344626739 ) ) ;
#18894 = VERTEX_POINT ( 'NONE', #5107 ) ;
#18895 = ORIENTED_EDGE ( 'NONE', *, *, #23462, .F. ) ;
#18896 = CARTESIAN_POINT ( 'NONE',  ( 43.06606138205700063, 42.19123852234595518, 61.30501292736988006 ) ) ;
#18897 = AXIS2_PLACEMENT_3D ( 'NONE', #21231, #17505, #23025 ) ;
#18898 = DIRECTION ( 'NONE',  ( 0.000000000000000000, -1.000000000000000000, 2.999999999999999839E-15 ) ) ;
#18899 = CARTESIAN_POINT ( 'NONE',  ( 37.69225076346193504, -15.81368208888610205, 72.33091598616826445 ) ) ;
#18900 = EDGE_LOOP ( 'NONE', ( #12094, #22986, #24612, #14830 ) ) ;
#18901 = VERTEX_POINT ( 'NONE', #22488 ) ;
#18902 = DIRECTION ( 'NONE',  ( 1.734723475976805122E-15, 2.999999999999999839E-15, 1.000000000000000000 ) ) ;
#18903 = CARTESIAN_POINT ( 'NONE',  ( 37.25202387243752611, -3.213682088886102406, 70.00779233799264034 ) ) ;
#18904 = CARTESIAN_POINT ( 'NONE',  ( 39.98359781491296161, -21.20384086642190979, 70.89533451361945993 ) ) ;
#18905 = VECTOR ( 'NONE', #20496, 1000.000000000000000 ) ;
#18906 = DIRECTION ( 'NONE',  ( 2.690219486203388234E-15, -0.8967398287344627850, -0.4425581086832399147 ) ) ;
#18907 = CARTESIAN_POINT ( 'NONE',  ( 36.07789103942398867, -1.413682088886102584, 70.70992431699450265 ) ) ;
#18908 = VECTOR ( 'NONE', #16856, 1000.000000000000000 ) ;
#18909 = DIRECTION ( 'NONE',  ( 1.327674326049719602E-15, -0.4425581086832399147, 0.8967398287344627850 ) ) ;
#18910 = ORIENTED_EDGE ( 'NONE', *, *, #8465, .F. ) ;
#18911 = CARTESIAN_POINT ( 'NONE',  ( 40.31606138205700773, -31.05876147765399864, 74.30501292737010033 ) ) ;
#18912 = EDGE_CURVE ( 'NONE', #20194, #3140, #15265, .T. ) ;
#18913 = EDGE_CURVE ( 'NONE', #20881, #8842, #17207, .T. ) ;
#18914 = DIRECTION ( 'NONE',  ( -1.000000000000000000, 0.000000000000000000, 0.000000000000000000 ) ) ;
#18915 = CARTESIAN_POINT ( 'NONE',  ( 40.56606138205697931, -5.948051402551118194, 9.959574150503843981 ) ) ;
#18916 = AXIS2_PLACEMENT_3D ( 'NONE', #17367, #9771, #21616 ) ;
#18917 = AXIS2_PLACEMENT_3D ( 'NONE', #8233, #2416, #2669 ) ;
#18918 = DIRECTION ( 'NONE',  ( 0.000000000000000000, 0.8212051873014208914, 0.5706330172266919076 ) ) ;
#18919 = DIRECTION ( 'NONE',  ( 1.000000000000000000, -0.000000000000000000, 0.000000000000000000 ) ) ;
#18920 = CARTESIAN_POINT ( 'NONE',  ( 30.81606138205697221, -3.542416608809866752, -4.744096181734387407 ) ) ;
#18921 = AXIS2_PLACEMENT_3D ( 'NONE', #11455, #8312, #18230 ) ;
#18922 = EDGE_LOOP ( 'NONE', ( #21835, #338, #25267, #14268 ) ) ;
#18923 = FACE_OUTER_BOUND ( 'NONE', #22297, .T. ) ;
#18924 = CARTESIAN_POINT ( 'NONE',  ( 33.31606138205700773, 3.296535697557910538, 65.33616386252352015 ) ) ;
#18925 = EDGE_LOOP ( 'NONE', ( #16179, #7591, #746, #17102 ) ) ;
#18926 = EDGE_LOOP ( 'NONE', ( #3812, #20291, #23359, #2887 ) ) ;
#18927 = CARTESIAN_POINT ( 'NONE',  ( 39.02088643472237806, -14.70384086642192045, 73.73360434286898624 ) ) ;
#18928 = AXIS2_PLACEMENT_3D ( 'NONE', #20668, #1068, #3637 ) ;
#18929 = DIRECTION ( 'NONE',  ( 0.000000000000000000, -0.7540134720837724513, -0.6568589528324737525 ) ) ;
#18930 = CARTESIAN_POINT ( 'NONE',  ( 36.80608444377001121, -19.31368208888609672, 70.35351908239857721 ) ) ;
#18931 = DIRECTION ( 'NONE',  ( -1.000000000000000000, 5.204170427930415223E-30, 1.734723475976805122E-15 ) ) ;
#18932 = VECTOR ( 'NONE', #20349, 1000.000000000000000 ) ;
#18933 =( NAMED_UNIT ( * ) PLANE_ANGLE_UNIT ( ) SI_UNIT ( $, .RADIAN. ) );
#18934 = ORIENTED_EDGE ( 'NONE', *, *, #11957, .T. ) ;
#18935 = LINE ( 'NONE', #10822, #10109 ) ;
#18936 = DIRECTION ( 'NONE',  ( -1.000000000000000000, 0.000000000000000000, 0.000000000000000000 ) ) ;
#18937 = CARTESIAN_POINT ( 'NONE',  ( 40.52078840805429394, 0.9961591335780859424, 72.15350918040385864 ) ) ;
#18938 = ORIENTED_EDGE ( 'NONE', *, *, #2203, .F. ) ;
#18939 = EDGE_CURVE ( 'NONE', #13262, #2806, #18441, .T. ) ;
#18940 =( NAMED_UNIT ( * ) PLANE_ANGLE_UNIT ( ) SI_UNIT ( $, .RADIAN. ) );
#18942 = EDGE_CURVE ( 'NONE', #1848, #1711, #18843, .T. ) ;
#18941 = CARTESIAN_POINT ( 'NONE',  ( 43.06606138205700063, -36.55876147765401640, 71.30501292737011454 ) ) ;
#18943 = CARTESIAN_POINT ( 'NONE',  ( 39.29254315202756231, -2.813682088886101162, 69.94417936956673998 ) ) ;
#18944 = CARTESIAN_POINT ( 'NONE',  ( 38.38987944808049235, -39.60718113818700203, 83.30501292737011454 ) ) ;
#18945 = EDGE_CURVE ( 'NONE', #17789, #21318, #19013, .T. ) ;
#18946 = CARTESIAN_POINT ( 'NONE',  ( 37.80618814713140097, -15.91368208888610880, 73.13360434286903455 ) ) ;
#18947 = LINE ( 'NONE', #13022, #1583 ) ;
#18948 = CARTESIAN_POINT ( 'NONE',  ( 31.81606138205700418, -33.00876147765401925, 70.30501292737011454 ) ) ;
#18949 = CARTESIAN_POINT ( 'NONE',  ( 39.24876120206129571, -18.90384086642191264, 72.12822762946747446 ) ) ;
#18950 = CARTESIAN_POINT ( 'NONE',  ( 37.33957961208646736, -7.813682088886109156, 72.81632618279323310 ) ) ;
#18951 = EDGE_LOOP ( 'NONE', ( #1484, #17190, #11423, #2438 ) ) ;
#18952 = CARTESIAN_POINT ( 'NONE',  ( 40.31606138205700773, -20.22127907754186893, 75.50705395623725735 ) ) ;
#18953 = EDGE_CURVE ( 'NONE', #21877, #12953, #15675, .T. ) ;
#18954 = ORIENTED_EDGE ( 'NONE', *, *, #9749, .T. ) ;
#18955 = CARTESIAN_POINT ( 'NONE',  ( 36.64852494920107517, -8.203840866421909794, 71.86517103874049894 ) ) ;
#18956 = DIRECTION ( 'NONE',  ( 1.000000000000000000, 2.999999999999999839E-15, 0.000000000000000000 ) ) ;
#18957 = CARTESIAN_POINT ( 'NONE',  ( 39.38009889167650357, 1.786317911113891821, 72.75271321436734695 ) ) ;
#18958 = VERTEX_POINT ( 'NONE', #14657 ) ;
#18959 = CARTESIAN_POINT ( 'NONE',  ( 39.12911128074873801, -10.11368208888610987, 73.69843995877330656 ) ) ;
#18960 = ORIENTED_EDGE ( 'NONE', *, *, #14726, .T. ) ;
#18961 = CARTESIAN_POINT ( 'NONE',  ( 43.81606138205700063, 7.166937456968672571, 6.752152658007350539 ) ) ;
#18962 = CARTESIAN_POINT ( 'NONE',  ( 37.31647492878124694, -12.30384086642191299, 72.03616607671141026 ) ) ;
#18963 = CARTESIAN_POINT ( 'NONE',  ( 38.31606138205700063, 39.69123852234598360, 71.30501292737018559 ) ) ;
#18964 = VECTOR ( 'NONE', #18546, 1000.000000000000000 ) ;
#18965 = ORIENTED_EDGE ( 'NONE', *, *, #8973, .T. ) ;
#18966 = LINE ( 'NONE', #1305, #10898 ) ;
#18967 = CYLINDRICAL_SURFACE ( 'NONE', #16164, 1.500000000000001332 ) ;
#18968 = CARTESIAN_POINT ( 'NONE',  ( 39.12911128074872380, -15.50384086642191228, 69.06206559358665231 ) ) ;
#18969 = VECTOR ( 'NONE', #2115, 1000.000000000000000 ) ;
#18970 = CARTESIAN_POINT ( 'NONE',  ( 36.51558096900348005, -21.10126295790812989, 75.36210271246490322 ) ) ;
#18971 = FILL_AREA_STYLE ('',( #10349 ) ) ;
#18972 = CARTESIAN_POINT ( 'NONE',  ( 39.82603832034400426, -18.31368208888610738, 72.40698646996133903 ) ) ;
#18973 = FACE_BOUND ( 'NONE', #21832, .T. ) ;
#18974 = CARTESIAN_POINT ( 'NONE',  ( 33.31606138205700773, -29.06829118875199924, 75.30501292737000085 ) ) ;
#18975 = ORIENTED_EDGE ( 'NONE', *, *, #14621, .T. ) ;
#18976 = DIRECTION ( 'NONE',  ( 0.000000000000000000, -2.999999999999999839E-15, -1.000000000000000000 ) ) ;
#18977 = DIRECTION ( 'NONE',  ( -1.327674326049719602E-15, 0.4425581086832399147, -0.8967398287344627850 ) ) ;
#18978 = CARTESIAN_POINT ( 'NONE',  ( 39.75915168707251723, -8.903840866421916189, 72.49904802271740323 ) ) ;
#18979 = PRODUCT_CONTEXT ( 'NONE', #11795, 'mechanical' ) ;
#18980 = DIRECTION ( 'NONE',  ( 1.000000000000000000, 0.000000000000000000, 0.000000000000000000 ) ) ;
#18981 = CARTESIAN_POINT ( 'NONE',  ( 38.26194895904383486, -25.01368208888610312, 69.64448340153876416 ) ) ;
#18982 = DIRECTION ( 'NONE',  ( 1.000000000000000000, -0.000000000000000000, 0.000000000000000000 ) ) ;
#18983 = EDGE_CURVE ( 'NONE', #2928, #19015, #18531, .T. ) ;
#18984 = VECTOR ( 'NONE', #11015, 1000.000000000000000 ) ;
#18985 = CARTESIAN_POINT ( 'NONE',  ( 39.95015449827720744, -23.00384086642191050, 71.96809898377887293 ) ) ;
#18986 = CARTESIAN_POINT ( 'NONE',  ( 37.42710149357921523, -5.407787168292675695, 83.30316041875967414 ) ) ;
#18987 = CARTESIAN_POINT ( 'NONE',  ( 36.49096545463212493, -21.51368208888609956, 71.43714994484034264 ) ) ;
#18988 = VERTEX_POINT ( 'NONE', #20981 ) ;
#18989 = CARTESIAN_POINT ( 'NONE',  ( 39.02088643472237806, 1.296159133578080658, 73.73360434286904308 ) ) ;
#18990 = ORIENTED_EDGE ( 'NONE', *, *, #24272, .F. ) ;
#18991 = CARTESIAN_POINT ( 'NONE',  ( 33.23058527440271348, 3.113468987225122220, 6.136968036621323286 ) ) ;
#18992 = DIRECTION ( 'NONE',  ( -1.000000000000000000, 5.204170427930415223E-30, 1.734723475976805122E-15 ) ) ;
#18993 = CARTESIAN_POINT ( 'NONE',  ( 38.63098279924288647, 1.086317911113899415, 70.22690120949094705 ) ) ;
#18994 = ORIENTED_EDGE ( 'NONE', *, *, #21377, .F. ) ;
#18995 = EDGE_LOOP ( 'NONE', ( #12419, #7014, #10380, #10826 ) ) ;
#18996 = DIRECTION ( 'NONE',  ( 0.000000000000000000, -1.000000000000000000, 2.999999999999999839E-15 ) ) ;
#18997 = DIRECTION ( 'NONE',  ( 1.000000000000000000, 2.999999999999999839E-15, 0.000000000000000000 ) ) ;
#18998 = ORIENTED_EDGE ( 'NONE', *, *, #17774, .T. ) ;
#18999 = DIRECTION ( 'NONE',  ( 1.000000000000000000, -0.000000000000000000, 0.000000000000000000 ) ) ;
#19000 = CARTESIAN_POINT ( 'NONE',  ( 37.33957961208645315, -3.803840866421909439, 69.94417936956673998 ) ) ;
#19001 = EDGE_CURVE ( 'NONE', #21641, #23726, #4874, .T. ) ;
#19002 = DIRECTION ( 'NONE',  ( -1.000000000000000000, 0.000000000000000000, 0.000000000000000000 ) ) ;
#19003 = ADVANCED_FACE ( 'NONE', ( #999 ), #860, .T. ) ;
#19004 = DIRECTION ( 'NONE',  ( -1.000000000000000000, 0.000000000000000000, 0.000000000000000000 ) ) ;
#19005 = EDGE_CURVE ( 'NONE', #16336, #8969, #1260, .T. ) ;
#19006 = VECTOR ( 'NONE', #11981, 1000.000000000000000 ) ;
#19007 = VERTEX_POINT ( 'NONE', #22896 ) ;
#19008 = ADVANCED_FACE ( 'NONE', ( #12999 ), #7199, .F. ) ;
#19009 = ORIENTED_EDGE ( 'NONE', *, *, #11627, .T. ) ;
#19010 = CARTESIAN_POINT ( 'NONE',  ( 33.88977883051490636, 3.189440311900809011, 6.370184205068262884 ) ) ;
#19011 = CARTESIAN_POINT ( 'NONE',  ( 38.82593461698262871, -2.913682088886100363, 69.62690120949091011 ) ) ;
#19012 = ORIENTED_EDGE ( 'NONE', *, *, #4768, .F. ) ;
#19013 = LINE ( 'NONE', #15014, #8984 ) ;
#19014 = CARTESIAN_POINT ( 'NONE',  ( 44.81606138205700063, 28.12806996228107437, 66.30501292736992980 ) ) ;
#19015 = VERTEX_POINT ( 'NONE', #9141 ) ;
#19016 = CARTESIAN_POINT ( 'NONE',  ( 30.81606138205697931, -31.26685248843966036, 43.18544225915084667 ) ) ;
#19017 = EDGE_CURVE ( 'NONE', #13333, #18144, #15042, .T. ) ;
#19018 = CARTESIAN_POINT ( 'NONE',  ( 30.17169630066736019, 1.361611432489138185, -2.592146606185724789 ) ) ;
#19019 = DIRECTION ( 'NONE',  ( -1.000000000000000000, 0.000000000000000000, 0.000000000000000000 ) ) ;
#19020 = ORIENTED_EDGE ( 'NONE', *, *, #20148, .F. ) ;
#19021 = AXIS2_PLACEMENT_3D ( 'NONE', #12673, #23775, #2261 ) ;
#19022 = LINE ( 'NONE', #24287, #21030 ) ;
#19023 = EDGE_LOOP ( 'NONE', ( #11927, #2932, #17484, #22103 ) ) ;
#19024 = ORIENTED_EDGE ( 'NONE', *, *, #11152, .F. ) ;
#19025 = CIRCLE ( 'NONE', #901, 0.7500000000000006661 ) ;
#19026 = LINE ( 'NONE', #1365, #10594 ) ;
#19027 = CARTESIAN_POINT ( 'NONE',  ( 43.31606138205700063, 7.187001342539796944, 66.09667597968754649 ) ) ;
#19028 = CARTESIAN_POINT ( 'NONE',  ( 39.41296390513587511, -16.41368208888610525, 71.67976084211551324 ) ) ;
#19029 = EDGE_LOOP ( 'NONE', ( #19009, #8950, #17373, #12759 ) ) ;
#19030 = ORIENTED_EDGE ( 'NONE', *, *, #2246, .F. ) ;
#19031 = AXIS2_PLACEMENT_3D ( 'NONE', #14148, #10665, #18145 ) ;
#19032 = DIRECTION ( 'NONE',  ( 1.927470528863119788E-16, 1.000000000000000000, -2.999999999999999839E-15 ) ) ;
#19033 = CARTESIAN_POINT ( 'NONE',  ( 40.14115730948191185, -23.10384086642191193, 71.43714994484030001 ) ) ;
#19034 = CARTESIAN_POINT ( 'NONE',  ( 42.82423818562821793, 3.225621635936315457, 6.370934609586303310 ) ) ;
#19035 = VECTOR ( 'NONE', #20487, 1000.000000000000114 ) ;
#19036 = CARTESIAN_POINT ( 'NONE',  ( 38.37017380507020192, -2.013682088886109334, 73.71602215082116061 ) ) ;
#19037 = EDGE_CURVE ( 'NONE', #4345, #4551, #7064, .T. ) ;
#19038 = EDGE_CURVE ( 'NONE', #23504, #11694, #22131, .T. ) ;
#19039 = VERTEX_POINT ( 'NONE', #2923 ) ;
#19040 = PLANE ( 'NONE',  #21111 ) ;
#19041 = CARTESIAN_POINT ( 'NONE',  ( 43.31606138205700063, -20.55619265724211076, 44.11584019928223910 ) ) ;
#19042 = AXIS2_PLACEMENT_3D ( 'NONE', #20820, #24656, #24408 ) ;
#19043 = CARTESIAN_POINT ( 'NONE',  ( 30.81606138205698286, -5.575886420685161049, -6.837621553846377154 ) ) ;
#19044 = FACE_OUTER_BOUND ( 'NONE', #25332, .T. ) ;
#19045 = DIRECTION ( 'NONE',  ( 1.000000000000000000, 0.000000000000000000, 0.000000000000000000 ) ) ;
#19046 = AXIS2_PLACEMENT_3D ( 'NONE', #11315, #7048, #23133 ) ;
#19047 = EDGE_CURVE ( 'NONE', #2631, #3300, #23964, .T. ) ;
#19048 = CARTESIAN_POINT ( 'NONE',  ( 35.31606138205700773, 7.864187680719676443, 65.89022736311019912 ) ) ;
#19049 = ORIENTED_EDGE ( 'NONE', *, *, #17138, .T. ) ;
#19050 = DIRECTION ( 'NONE',  ( -1.000000000000000000, 0.000000000000000000, 0.000000000000000000 ) ) ;
#19051 = VECTOR ( 'NONE', #9763, 1000.000000000000227 ) ;
#19052 = CARTESIAN_POINT ( 'NONE',  ( 40.10895460087045450, 5.898345303533535144, 65.30501292737000085 ) ) ;
#19053 = ORIENTED_EDGE ( 'NONE', *, *, #12599, .F. ) ;
#19054 = ORIENTED_EDGE ( 'NONE', *, *, #19713, .F. ) ;
#19055 = UNCERTAINTY_MEASURE_WITH_UNIT (LENGTH_MEASURE( 1.000000000000000082E-05 ), #13232, 'distance_accuracy_value', 'NONE');
#19056 = CARTESIAN_POINT ( 'NONE',  ( 36.89935272106205133, -12.40384086642192152, 73.23812341099225875 ) ) ;
#19057 = EDGE_CURVE ( 'NONE', #15655, #8846, #6339, .T. ) ;
#19058 = CIRCLE ( 'NONE', #10418, 0.7500000000000006661 ) ;
#19059 = DIRECTION ( 'NONE',  ( -2.480932259201170508E-15, 0.9193606199277819524, 0.3934158747763039088 ) ) ;
#19060 = CARTESIAN_POINT ( 'NONE',  ( 39.75915168707250302, -20.71368208888610596, 70.26145752964251301 ) ) ;
#19061 = ORIENTED_EDGE ( 'NONE', *, *, #25294, .F. ) ;
#19062 = DIRECTION ( 'NONE',  ( 1.000000000000000000, 0.000000000000000000, -0.000000000000000000 ) ) ;
#19063 = CARTESIAN_POINT ( 'NONE',  ( 36.31606138205700063, -10.19550266980813369, 14.63954348514304904 ) ) ;
#19064 = CIRCLE ( 'NONE', #1755, 0.2000000000000057288 ) ;
#19065 = CARTESIAN_POINT ( 'NONE',  ( 40.33642880535524000, -24.31368208888611093, 72.77780686321125359 ) ) ;
#19066 = ORIENTED_EDGE ( 'NONE', *, *, #4827, .F. ) ;
#19067 = DIRECTION ( 'NONE',  ( 1.000000000000000000, -0.000000000000000000, 0.000000000000000000 ) ) ;
#19068 = LINE ( 'NONE', #9411, #4509 ) ;
#19069 = LINE ( 'NONE', #3211, #10551 ) ;
#19070 = VECTOR ( 'NONE', #4564, 1000.000000000000000 ) ;
#19071 = CARTESIAN_POINT ( 'NONE',  ( 36.49096545463212493, -13.51368208888610489, 71.43714994484034264 ) ) ;
#19072 = CARTESIAN_POINT ( 'NONE',  ( 43.81606138205700063, 22.19123852234701388, 73.80501292736992980 ) ) ;
#19073 = AXIS2_PLACEMENT_3D ( 'NONE', #22292, #4655, #12533 ) ;
#19074 = DIRECTION ( 'NONE',  ( -1.000000000000000000, -1.956963323498894821E-16, 5.870889970496684443E-31 ) ) ;
#19075 = CARTESIAN_POINT ( 'NONE',  ( 37.21915885897815457, -16.20384086642190979, 71.67976084211552745 ) ) ;
#19076 = CARTESIAN_POINT ( 'NONE',  ( 37.80618814713140097, -5.913682088886107024, 73.13360434286904876 ) ) ;
#19077 = ORIENTED_EDGE ( 'NONE', *, *, #14606, .F. ) ;
#19078 = CARTESIAN_POINT ( 'NONE',  ( 39.33009355364794146, -21.96558760913888264, 75.30775939357174309 ) ) ;
#19079 = AXIS2_PLACEMENT_3D ( 'NONE', #25373, #3496, #17163 ) ;
#19080 = LINE ( 'NONE', #10498, #1624 ) ;
#19081 = ORIENTED_EDGE ( 'NONE', *, *, #23270, .T. ) ;
#19082 = ORIENTED_EDGE ( 'NONE', *, *, #18472, .T. ) ;
#19083 = EDGE_CURVE ( 'NONE', #14416, #10854, #4404, .T. ) ;
#19084 = CARTESIAN_POINT ( 'NONE',  ( 40.55423172469004101, -29.20384086642191335, 70.70992431699446001 ) ) ;
#19085 = DIRECTION ( 'NONE',  ( 1.000000000000000000, 0.000000000000000000, 0.000000000000000000 ) ) ;
#19086 = EDGE_CURVE ( 'NONE', #21114, #1537, #5001, .T. ) ;
#19087 = AXIS2_PLACEMENT_3D ( 'NONE', #17524, #23555, #4120 ) ;
#19088 = CARTESIAN_POINT ( 'NONE',  ( 36.87297107704152666, 0.2863179111138939303, 72.49904802271743165 ) ) ;
#19089 = CARTESIAN_POINT ( 'NONE',  ( 40.33642880535524000, -10.31368208888610738, 72.77780686321128201 ) ) ;
#19090 = ORIENTED_EDGE ( 'NONE', *, *, #12633, .T. ) ;
#19091 = LINE ( 'NONE', #18961, #2070 ) ;
#19092 = CARTESIAN_POINT ( 'NONE',  ( 37.60469502381300799, -8.403840866421912636, 72.26730301774236409 ) ) ;
#19093 = COLOUR_RGB ( '', 0.66274510, 0.83137255, 0.94901961) ;
#19094 = FILL_AREA_STYLE ('',( #13544 ) ) ;
#19095 = ORIENTED_EDGE ( 'NONE', *, *, #3131, .F. ) ;
#19096 = CARTESIAN_POINT ( 'NONE',  ( 44.06606138205700063, 42.82479937715250173, 82.59790614618329130 ) ) ;
#19097 = CARTESIAN_POINT ( 'NONE',  ( 35.56606138205700063, -13.51824891481310509, 37.72654391001022134 ) ) ;
#19098 = CARTESIAN_POINT ( 'NONE',  ( 36.36258059203030513, -7.903840866421910860, 69.89063713639259845 ) ) ;
#19099 = VECTOR ( 'NONE', #2722, 1000.000000000000000 ) ;
#19100 = CARTESIAN_POINT ( 'NONE',  ( 37.31068429205632953, -21.95526386996113999, 75.30827953495455063 ) ) ;
#19101 =( NAMED_UNIT ( * ) PLANE_ANGLE_UNIT ( ) SI_UNIT ( $, .RADIAN. ) );
#19102 = CARTESIAN_POINT ( 'NONE',  ( 38.26194895904383486, -21.01368208888610312, 69.64448340153877837 ) ) ;
#19103 = DIRECTION ( 'NONE',  ( -1.000000000000000000, 1.115179377413661005E-30, 3.717264591378870232E-16 ) ) ;
#19104 = EDGE_CURVE ( 'NONE', #9423, #17658, #10804, .T. ) ;
#19105 = VECTOR ( 'NONE', #2509, 1000.000000000000000 ) ;
#19106 = DIRECTION ( 'NONE',  ( 1.000000000000000000, 2.999999999999999839E-15, 0.000000000000000000 ) ) ;
#19107 = ORIENTED_EDGE ( 'NONE', *, *, #11536, .T. ) ;
#19108 = DIRECTION ( 'NONE',  ( -2.048868001712898319E-15, 0.6595716529892350355, -0.7516416929448821449 ) ) ;
#19109 = CARTESIAN_POINT ( 'NONE',  ( 39.82603832034401137, -11.30384086642190944, 70.35351908239860563 ) ) ;
#19110 = APPLICATION_PROTOCOL_DEFINITION ( 'draft international standard', 'automotive_design', 1998, #15387 ) ;
#19111 = CARTESIAN_POINT ( 'NONE',  ( 33.56606138205700773, -34.55876147765400930, 73.55501292737011454 ) ) ;
#19112 = CARTESIAN_POINT ( 'NONE',  ( 39.75915168707250302, -22.71368208888610241, 70.26145752964251301 ) ) ;
#19113 = DIRECTION ( 'NONE',  ( -1.000000000000000000, 0.000000000000000000, 0.000000000000000000 ) ) ;
#19114 = VECTOR ( 'NONE', #13334, 1000.000000000000000 ) ;
#19115 = CARTESIAN_POINT ( 'NONE',  ( 38.93415946300896024, -21.50384086642190340, 69.66206559358661821 ) ) ;
#19116 = CARTESIAN_POINT ( 'NONE',  ( 38.05217264712879199, -5.217360829629674512, 83.31008614951315394 ) ) ;
#19117 = CARTESIAN_POINT ( 'NONE',  ( 38.37017380507020192, -16.01368208888610667, 73.11602215082116629 ) ) ;
#19118 = VERTEX_POINT ( 'NONE', #16592 ) ;
#19119 = CARTESIAN_POINT ( 'NONE',  ( 37.50301148336529877, -0.5038408664219187205, 73.69843995877330656 ) ) ;
#19120 = ORIENTED_EDGE ( 'NONE', *, *, #14483, .T. ) ;
#19121 = CARTESIAN_POINT ( 'NONE',  ( 30.81606138205696865, -3.028410647649177889, 0.3252050635115383281 ) ) ;
#19122 = CARTESIAN_POINT ( 'NONE',  ( 38.31606138205700063, -30.30876147765401285, 71.30501292737010033 ) ) ;
#19123 = CARTESIAN_POINT ( 'NONE',  ( 39.37952058850012804, -27.00384086642191050, 71.78268878715390144 ) ) ;
#19124 = ORIENTED_EDGE ( 'NONE', *, *, #19946, .T. ) ;
#19125 = ORIENTED_EDGE ( 'NONE', *, *, #8624, .T. ) ;
#19126 = CARTESIAN_POINT ( 'NONE',  ( 43.77578593420113862, 3.724120516973108419, 6.250574242801828717 ) ) ;
#19127 = DIRECTION ( 'NONE',  ( -1.000000000000000000, -2.999999999999999839E-15, 0.000000000000000000 ) ) ;
#19128 = FACE_OUTER_BOUND ( 'NONE', #22244, .T. ) ;
#19129 = CARTESIAN_POINT ( 'NONE',  ( 37.69796330110505522, -2.503840866421913613, 73.09843995877331224 ) ) ;
#19130 = LINE ( 'NONE', #8966, #16621 ) ;
#19131 = ORIENTED_EDGE ( 'NONE', *, *, #18398, .F. ) ;
#19132 = EDGE_CURVE ( 'NONE', #9471, #23179, #15816, .T. ) ;
#19133 = FACE_OUTER_BOUND ( 'NONE', #13071, .T. ) ;
#19134 = AXIS2_PLACEMENT_3D ( 'NONE', #13674, #21272, #3880 ) ;
#19135 = EDGE_LOOP ( 'NONE', ( #15332, #5462, #13608, #6247, #17070, #15226, #18637, #18866, #21971, #18824, #23057, #2875 ) ) ;
#19136 = ORIENTED_EDGE ( 'NONE', *, *, #4724, .F. ) ;
#19137 = DIRECTION ( 'NONE',  ( 0.9835979625596965592, -0.1803747433772641684, -2.086002012065537230E-15 ) ) ;
#19138 = CARTESIAN_POINT ( 'NONE',  ( 39.38009889167650357, -4.213682088886106847, 72.75271321436733274 ) ) ;
#19139 = CARTESIAN_POINT ( 'NONE',  ( 37.69796330110505522, -24.50384086642191406, 73.09843995877328382 ) ) ;
#19140 = LINE ( 'NONE', #7547, #5469 ) ;
#19141 =( BOUNDED_SURFACE ( )  B_SPLINE_SURFACE ( 3, 2, ( 
 ( #16031, #10121, #21963, #17979, #6382, #12313, #23882, #12445, #9868, #12190, #20159, #10627, #6623, #12945, #5080, #4947, #18479, #14484, #8568, #18858, #4814, #22845, #20797, #3132, #18355, #4701, #12693, #813, #22717, #10758, #5206, #20665, #24502, #13068, #10502, #2998, #8700, #16531, #11002, #14992, #2624, #20534, #16793, #1197, #6756, #2867, #9085, #12575, #22341, #680, #24253, #16405, #8948, #10880, #20406, #24626, #2739, #18598, #24382, #14609, #22464, #939, #16928, #1065, #8831, #24759, #16669, #7006, #7138, #6876, #14730, #22592, #12817, #18733, #14855, #18987, #19230, #17182, #5333, #13324, #11520, #9711, #19359, #7261, #23216, #1694, #25006, #7775, #25266, #21175, #17562, #1568, #5706, #19485, #11389, #15488, #15619, #9461, #5835, #3260, #23340, #17310, #20919, #7396, #1328, #15240, #3633, #11135, #9214, #13569, #17063, #21421, #25132, #24882, #23093, #15112, #5454, #9589, #22969, #13198, #3765, #9336, #25390, #3391, #3514, #11648, #21049, #1828, #11271, #23470, #19117, #7518, #15366, #7647, #1456, #5583, #13441, #21292, #17439, #19874, #3902, #17951, #11899, #6218, #10212, #19740, #8411, #14210, #2083, #13946, #21675, #17691, #23974, #16122, #15994, #4026, #21, #19608, #4414, #15872, #16251, #6351, #22050, #11776, #15750, #23725, #9964, #8279, #21803, #24096, #14076, #10093, #13696, #21554, #21930, #17823, #153, #12281, #527, #1951, #6091, #2336, #20123, #8032, #4161, #2458, #23605, #7903, #9834, #5967, #13817, #19996, #4292, #12031, #18075, #2213, #271, #8150, #23845, #12160, #397, #10336, #18199, #20378, #1035, #10472, #20631, #24594, #14326, #18823, #14451, #6718, #4782, #4915, #4544, #12661, #2708, #16369, #24344, #22560, #20767, #12787, #18327, #8795, #2966, #10596, #1161, #10851, #14574, #3097, #20503, #16760, #5042, #22432, #8916, #9054, #2835, #16895, #6593, #18700, #12408, #10724, #22179, #12914, #6842, #4664, #24469, #18447, #20249, #18570, #6976, #6469, #777, #2587, #651, #905, #8536, #22305, #10970, #24217, #8669, #14827, #12542, #14698, #22685, #16499, #16633, #5179, #19203, #15207, #13164, #17028, #24858, #13414, #14959, #21144, #20888, #9431, #9310, #11361, #11102, #17276, #3735, #7358, #7235, #21394, #3359, #1427, #1796, #23308, #7104, #17404, #22817, #19088, #25237, #17152, #13032, #21017, #5553, #15081, #3488, #23187, #1661, #21262, #7482, #22935, #19454, #5299, #18957, #9688, #15338 ),
 ( #23059, #11236, #9182, #24979, #3607, #13538, #11490, #1295, #1541, #19330, #5425, #11611, #9554, #13294, #24728, #25101, #7620, #5675, #15461, #3224, #12609, #8006, #2779, #25360, #12484, #13921, #17537, #21645, #15587, #3997, #603, #7746, #23444, #10541, #5936, #22380, #4332, #19709, #18391, #19583, #722, #5810, #24292, #8605, #6061, #21776, #2057, #20447, #16444, #2660, #13666, #1921, #9934, #7875, #20328, #124, #21522, #10410, #4134, #3870, #11748, #18275, #15720, #13792, #6660, #4736, #9808, #17792, #6537, #14522, #11875, #15842, #17664, #23573, #23696, #12003, #19842, #2530, #24162, #8480, #16314, #14396, #22250, #4610, #4857, #22504, #20574, #12731, #5244, #9124, #24539, #13111, #14644, #24799, #3303, #18515, #23008, #18640, #10920, #8990, #16966, #8736, #16838, #6920, #2904, #3042, #1243, #24919, #7180, #10789, #12985, #15028, #14773, #5373, #22883, #18769, #7304, #24673, #20962, #9256, #1104, #11178, #13239, #7045, #21089, #845, #19028, #14896, #10669, #22631, #16572, #4987, #18899, #24422, #6795, #1369, #12851, #15154, #980, #20706, #17100, #8868, #16706, #22755, #5124, #20833, #3172, #11042, #7814, #15280, #15659, #9631, #19654, #13612, #17483, #19152, #7684, #1610, #21461, #25432, #9502, #23648, #3942, #17347, #3678, #11429, #7432, #13738, #5877, #5746, #19272, #23129, #9375, #1992, #1488, #25309, #25046, #3805, #13481, #15531, #5501, #11691, #7946, #11560, #3550, #62, #7564, #5618, #6006, #9875, #11312, #21595, #17224, #23257, #11813, #21330, #13365, #25172, #9752, #21211, #23379, #1866, #17731, #23508, #19530, #15414, #13859, #19397, #1733, #3434, #17603, #15790, #8321, #12068, #6388, #20165, #14244, #2376, #2501, #10375, #6630, #18362, #22089, #18242, #18118, #8577, #16160, #21841, #313, #16038, #16412, #2630, #21717, #21969, #24131, #23890, #16284, #13992, #11943, #10001, #24260, #22219, #17865, #567, #4198, #23767, #6254, #24013, #189, #4454, #14117, #2120, #2253, #687, #17988, #4072, #20296, #19783, #4333, #8192, #8069, #6508, #19915, #12322, #15909, #10508, #10127, #8449, #6132, #10252, #12196, #20034, #14365, #440, #4584, #12451, #22348, #2874, #1073, #12951, #22471, #4707, #2745, #16676, #14490, #14615, #3138, #20412, #20541, #18739, #20803, #12823, #8954, #10764, #10886, #10636, #4955, #8837, #12701, #24389, #6763, #16800, #24633, #7013, #12582, #18486, #14861, #22723, #20671, #820, #5087 ),
 ( #8706, #18604, #4820, #946, #16537, #24508, #3005, #6882, #14738, #22599, #6342, #6460, #8141, #4535, #4406, #17945, #18067, #8661, #8273, #24336, #10583, #2208, #12274, #16113, #15986, #6585, #4284, #20239, #16492, #18439, #12154, #24209, #10086, #18190, #263, #770, #12400, #10205, #2578, #23967, #23840, #20117, #14445, #6708, #14202, #6211, #14068, #24089, #12023, #19991, #14566, #19865, #22045, #10462, #22423, #18321, #640, #2451, #8524, #21922, #14318, #10329, #389, #2327, #520, #16361, #8405, #16243, #22172, #22293, #4656, #12534, #20370, #2701, #9301, #12904, #4904, #1417, #8910, #6968, #7348, #3349, #12653, #22925, #20492, #24585, #5286, #14819, #2827, #18692, #11093, #22552, #1151, #3215, #7226, #1288, #13025, #2956, #24967, #10841, #16623, #15195, #20877, #10718, #16888, #20624, #14951, #18949, #22808, #10961, #16750, #9171, #11225, #5170, #17018, #22677, #24851, #18563, #24719, #20758, #1026, #12781, #5033, #15071, #894, #9044, #8787, #13155, #3091, #7093, #24463, #21007, #17142, #18814, #19075, #4774, #6835, #14687, #112, #21636, #5416, #15710, #13283, #17394, #23561, #25227, #21134, #11479, #3861, #15326, #19441, #21511, #25487, #19574, #5800, #21253, #17784, #3597, #9420, #7996, #13658, #3477, #9679, #13405, #7732, #11740, #15576, #3726, #1913, #9797, #23051, #19699, #23435, #17652, #1787, #9926, #17528, #23177, #1653, #7611, #11352, #3988, #19195, #23297, #7867, #15453, #5927, #5545, #1529, #17266, #25091, #13784, #7474, #11864, #19319, #9544, #5663, #25352, #13528, #2047, #21382, #11603, #19773, #21705, #181, #7677, #19388, #13604, #4059, #13471, #11932, #17339, #17855, #2112, #25420, #7805, #15782, #23249, #23638, #17594, #9993, #21586, #15652, #1601, #23500, #9623, #3935, #7936, #17474, #6121, #8059, #25299, #11681, #1723, #15404, #15900, #13851, #25163, #15519, #13728, #7555, #23756, #13980, #9491, #19522, #23371, #5609, #5997, #3667, #19642, #21833, #11419, #11553, #19263, #21322, #5869, #5737, #21454, #11805, #3795, #1982, #1858, #9743, #9865, #17723, #54, #8311, #19905, #16027, #16275, #4189, #12186, #8697, #12059, #16149, #2619, #10624, #22207, #10499, #24001, #20284, #10118, #24121, #20154, #18107, #21959, #4323, #18352, #2243, #557, #301, #14355, #14235, #6496, #23878, #4574, #16528, #12309, #20025, #808, #6379, #22078, #6752, #2736, #17976, #22337, #8181, #4442, #4696, #2491, #6245 ),
 ( #24376, #10240, #14105, #14605, #12442, #2363, #677, #429, #8565, #16400, #24248, #10365, #6620, #14480, #18229, #8438, #12571, #20403, #18475, #9334, #16926, #22588, #1063, #16790, #17180, #3388, #7392, #22715, #24880, #24623, #17060, #14728, #12690, #10754, #25004, #22967, #18595, #11131, #4944, #24498, #7004, #24757, #935, #14989, #14853, #22460, #15110, #7259, #20530, #6872, #5076, #12815, #5330, #12942, #4811, #22843, #18855, #2863, #8826, #5204, #20662, #10878, #13195, #16666, #2996, #20795, #18985, #21045, #8945, #3129, #11266, #18730, #11000, #1193, #9082, #7136, #3256, #13066, #20917, #1325, #9211, #19115, #1454, #1566, #25127, #17307, #9832, #13693, #3631, #17687, #19228, #3898, #7900, #23089, #2079, #23214, #15486, #13566, #21552, #13321, #21418, #11517, #7514, #7645, #5833, #4023, #11773, #9458, #17560, #19605, #19357, #9961, #1949, #23337, #11897, #3762, #18, #13813, #5704, #15747, #17820, #11644, #151, #5451, #23602, #19480, #15236, #1690, #21173, #9584, #23467, #3512, #5964, #21671, #19737, #17435, #5581, #25263, #11387, #15362, #13438, #21290, #1825, #9709, #25388, #7772, #15616, #19871, #20246, #14207, #24215, #18195, #22048, #23719, #12278, #6215, #524, #4541, #14073, #2706, #8532, #21927, #8276, #15991, #12028, #18325, #10469, #10333, #23843, #2211, #13944, #6591, #10210, #2583, #20376, #12158, #6088, #10090, #20121, #8031, #4289, #12538, #15869, #19994, #6466, #14449, #8408, #14324, #2332, #24093, #21801, #2455, #23971, #18071, #267, #8146, #22177, #4158, #4410, #17949, #16248, #393, #12404, #16119, #647, #10590, #6346, #16367, #4661, #22299, #18445, #3357, #24856, #8666, #18955, #16497, #20628, #1293, #2962, #24341, #14694, #7101, #18568, #22683, #24725, #3222, #22814, #9051, #24467, #21014, #6839, #12657, #11233, #16893, #6713, #12911, #16628, #10966, #14957, #18819, #6974, #5177, #13030, #775, #22931, #1158, #20883, #5039, #13162, #20764, #902, #4911, #10848, #14571, #7232, #22429, #1031, #11099, #18697, #9178, #8793, #4780, #20499, #2833, #17025, #10722, #15079, #22558, #12785, #8914, #3095, #16755, #5294, #24592, #14824, #25098, #21392, #7356, #7874, #9805, #9308, #19329, #23186, #15204, #13665, #11360, #1795, #15718, #17661, #19202, #5808, #17150, #25235, #24977, #7179, #19450, #17275, #11610, #15335, #23058, #1660, #11488, #9686, #23571, #17536, #5423, #3734, #25359, #5552, #5935, #23443 ),
 ( #3995, #1425, #21520, #15460, #19084, #13413, #13292, #21261, #7741, #21142, #1920, #3869, #13791, #3605, #1538, #9551, #11747, #3485, #19581, #9430, #21643, #7481, #7619, #23305, #17402, #5672, #13536, #15585, #2557, #22024, #18045, #2056, #16094, #10063, #4386, #8381, #17923, #6561, #12381, #240, #12131, #19841, #15841, #22146, #14296, #14182, #2183, #23695, #17791, #10439, #14045, #14423, #4508, #20220, #9933, #13917, #21900, #8120, #6441, #19972, #22274, #12248, #8251, #11873, #19707, #20091, #15963, #23818, #18300, #24189, #121, #4263, #495, #622, #6194, #2304, #8506, #21774, #6060, #8005, #4133, #12002, #18171, #2431, #10178, #16223, #365, #23944, #6318, #10310, #24073, #16337, #24701, #3070, #18543, #7072, #8633, #18794, #22786, #12513, #16996, #12630, #4881, #2934, #10943, #2681, #10815, #870, #14546, #16731, #16468, #14799, #9150, #12760, #4755, #1270, #8762, #6819, #7209, #3196, #20352, #5149, #10563, #24446, #13007, #14665, #18419, #16600, #1131, #22405, #1008, #9018, #14926, #16865, #12882, #2808, #24829, #10695, #24314, #15050, #20735, #747, #24562, #20471, #22660, #20857, #5012, #18668, #11071, #18927, #4634, #6685, #22528, #20603, #8891, #6944, #17374, #23032, #1512, #17247, #9778, #3837, #7845, #23156, #25333, #25071, #17510, #15177, #13135, #11205, #25464, #23408, #19056, #11588, #5399, #24945, #7458, #25203, #1400, #15436, #15307, #3330, #3460, #7593, #9281, #11721, #13638, #20988, #5530, #9399, #17126, #7714, #13263, #5644, #19557, #21492, #21116, #9660, #7329, #3577, #11337, #1892, #23285, #19177, #13509, #13392, #21237, #11459, #15556, #17635, #19297, #1634, #9530, #21358, #22907, #3704, #5269, #19420, #1765, #5776, #22122, #8223, #22003, #19814, #6291, #21622, #10156, #6162, #4105, #7977, #15820, #4359, #5908, #12102, #11844, #341, #220, #12222, #13769, #8097, #9906, #2027, #91, #17762, #10284, #14149, #11977, #18146, #19682, #20068, #8354, #23538, #2529, #23675, #15940, #14021, #2405, #3970, #21876, #2153, #6036, #23793, #470, #4486, #16196, #13891, #18021, #24046, #10033, #10409, #6420, #4230, #12354, #19944, #14270, #20196, #2280, #18274, #602, #16068, #15689, #21745, #17897, #23919, #19232, #12608, #6535, #20444, #17065, #8476, #17184, #19119, #23095, #4735, #16442, #10666, #1458, #10540, #9338, #14394, #15242, #25008, #22500, #4855, #13200, #20327, #21051, #14642, #7398, #18989, #13070 ),
 ( #8735, #24291, #12483, #5456, #11273, #11137, #6658, #2659, #22248, #13326, #18514, #3516, #21177, #11391, #24161, #18386, #844, #14521, #3393, #16569, #16311, #1330, #20921, #4609, #720, #9216, #22378, #2776, #8603, #24420, #6793, #3262, #22971, #24884, #7263, #15114, #5335, #11522, #13443, #17312, #23218, #12033, #7905, #19610, #3635, #7520, #13698, #17441, #11778, #23, #1953, #7777, #15752, #23607, #1570, #23727, #9836, #5969, #23472, #13948, #21556, #1696, #5708, #21423, #21805, #8034, #9463, #1830, #4028, #3767, #21677, #19361, #25134, #15368, #4163, #2085, #5585, #13819, #9591, #25268, #11650, #3904, #21294, #17693, #19487, #7649, #15490, #11901, #23342, #15874, #17825, #13571, #9713, #17564, #25392, #19742, #15621, #9966, #6093, #155, #5837, #6595, #17953, #529, #10095, #779, #20251, #18077, #12410, #16124, #273, #20125, #14453, #6720, #23976, #8152, #6220, #6471, #19876, #2338, #24346, #2215, #6353, #18329, #8671, #2589, #653, #14212, #10474, #15996, #14328, #10338, #8281, #12162, #19998, #8538, #23847, #16253, #14078, #4546, #4416, #22181, #21932, #16371, #14576, #2461, #10214, #16501, #22052, #12283, #22434, #18449, #4294, #12544, #399, #18201, #20380, #8413, #24098, #24219, #22307, #4666, #2710, #10598, #4784, #9184, #20890, #10853, #7359, #18702, #24471, #23061, #3226, #2837, #12916, #7237, #24980, #16762, #10726, #6844, #24730, #12663, #20633, #17153, #20505, #24596, #11104, #19089, #5181, #18959, #6978, #1297, #18572, #7106, #3100, #1037, #4917, #12789, #17030, #907, #9056, #8797, #22819, #22687, #14961, #14700, #13034, #15208, #20769, #2968, #9312, #14829, #5044, #16635, #11238, #22562, #5301, #8918, #10972, #13166, #18825, #1163, #16897, #24860, #15083, #22937, #21020, #3361, #1428, #13667, #3608, #125, #11491, #17277, #15843, #21523, #11363, #17539, #21263, #15588, #3871, #23445, #11612, #11749, #19585, #5426, #2058, #5811, #1922, #1797, #17793, #25361, #5554, #9555, #25238, #8007, #11876, #13295, #5676, #7877, #7621, #3877, #23188, #21145, #19204, #3489, #5937, #1542, #9809, #13416, #7483, #15462, #7747, #9432, #17665, #23309, #25102, #19331, #15721, #15339, #19710, #21647, #1663, #13539, #17405, #21395, #23574, #3737, #13793, #9936, #3998, #19455, #9689, #21777, #4389, #13922, #4635, #24074, #21902, #16225, #19974, #8383, #22148, #6444, #12249, #4510, #12382, #8637, #20353, #14298, #20221 ),
 ( #23945, #624, #367, #18301, #15965, #4135, #12005, #751, #24191, #19843, #2559, #23821, #241, #18047, #18174, #2186, #10441, #16096, #10065, #4265, #496, #17924, #12515, #14424, #8121, #6321, #2306, #6195, #8507, #14047, #16340, #2682, #22275, #12134, #6563, #10179, #20093, #8253, #10565, #18420, #14183, #23698, #22027, #2433, #10311, #6062, #3332, #20606, #6686, #2810, #3071, #16469, #24447, #20992, #24315, #2936, #14930, #22909, #9020, #22790, #10817, #7073, #22407, #10944, #6946, #4884, #8763, #16602, #5150, #14548, #12885, #12631, #1133, #1009, #18795, #10700, #16867, #11207, #24563, #6820, #13138, #18670, #8892, #19060, #15052, #4756, #9153, #20473, #16733, #16999, #14802, #18545, #12762, #13008, #14666, #20737, #20858, #18930, #3197, #24703, #22529, #1403, #22661, #871, #5015, #11075, #1272, #24833, #7212, #5271, #21119, #11590, #7718, #5533, #21625, #13641, #9532, #23542, #7596, #19560, #7851, #25207, #3841, #3973, #15438, #19685, #17129, #11724, #5646, #9285, #13395, #7331, #21239, #17513, #24947, #17639, #1895, #5911, #3580, #17250, #11462, #9781, #11339, #25468, #15180, #15693, #13772, #23287, #13513, #21495, #3464, #11847, #21362, #23036, #19423, #3706, #5402, #1769, #7460, #9665, #5781, #15310, #13265, #19181, #23158, #17376, #25074, #1515, #9401, #19300, #25336, #1637, #15559, #23414, #18279, #4236, #22255, #20201, #12360, #17768, #4109, #12107, #10036, #22125, #10159, #4615, #20071, #23923, #12489, #9910, #2410, #223, #15943, #10415, #14400, #2031, #19948, #16199, #607, #6165, #2283, #8484, #11982, #13894, #96, #23678, #7981, #8358, #10288, #19819, #24051, #15823, #18025, #21749, #2159, #17900, #8100, #4490, #474, #23797, #2535, #6039, #6424, #16318, #14025, #21881, #344, #8227, #16072, #14274, #6296, #14155, #22008, #4363, #12225, #18150, #24166, #6541, #22384, #14648, #14777, #16448, #12857, #12735, #726, #850, #22635, #8610, #9128, #11046, #10546, #20578, #24426, #24297, #14901, #12613, #3046, #16972, #18903, #20452, #7049, #18395, #984, #6665, #1247, #20711, #18519, #10925, #16577, #14527, #2911, #22761, #7185, #6799, #4740, #2783, #6925, #20332, #10673, #24805, #2664, #22508, #18773, #15032, #1109, #8994, #4861, #16842, #8741, #4991, #10794, #18645, #8872, #16710, #24677, #24543, #5128, #12989, #20838, #3176, #22887, #5249, #23263, #17609, #21216, #13244, #9758, #17228, #15284, #15666, #11698 ) ),
 .UNSPECIFIED., .T., .F., .F. ) 
 B_SPLINE_SURFACE_WITH_KNOTS ( ( 4, 3, 4 ),
 ( 3, 2, 2, 2, 2, 2, 2, 2, 2, 2, 2, 2, 2, 2, 2, 2, 2, 2, 2, 2, 2, 2, 2, 2, 2, 2, 2, 2, 2, 2, 2, 2, 2, 2, 2, 2, 2, 2, 2, 2, 2, 2, 2, 2, 2, 2, 2, 2, 2, 2, 2, 2, 2, 2, 2, 2, 2, 2, 2, 2, 2, 2, 2, 2, 2, 2, 2, 2, 2, 2, 2, 2, 2, 2, 2, 2, 2, 2, 2, 2, 2, 2, 2, 2, 2, 2, 2, 2, 2, 2, 2, 2, 2, 2, 2, 2, 2, 2, 2, 2, 2, 2, 2, 2, 2, 2, 2, 2, 2, 2, 2, 2, 2, 2, 2, 2, 2, 2, 2, 2, 2, 2, 2, 2, 2, 2, 2, 2, 2, 2, 2, 2, 2, 2, 2, 2, 2, 2, 2, 2, 2, 2, 2, 2, 2, 2, 2, 2, 2, 2, 2, 2, 2, 2, 2, 3 ),
 ( 0.000000000000000000, 0.5000000000000000000, 1.000000000000000000 ),
 ( 0.000000000000000000, 0.006250000000000000347, 0.01250000000000000069, 0.01874999999999999931, 0.02500000000000000139, 0.03125000000000000000, 0.03749999999999999861, 0.04374999999999999722, 0.05000000000000000278, 0.05625000000000000139, 0.06250000000000000000, 0.06875000000000000555, 0.07499999999999999722, 0.08125000000000000278, 0.08749999999999999445, 0.09375000000000000000, 0.1000000000000000056, 0.1062499999999999972, 0.1125000000000000028, 0.1187499999999999944, 0.1250000000000000000, 0.1312500000000000056, 0.1375000000000000111, 0.1437499999999999889, 0.1499999999999999944, 0.1562500000000000000, 0.1625000000000000056, 0.1687500000000000111, 0.1749999999999999889, 0.1812499999999999944, 0.1875000000000000000, 0.1937500000000000056, 0.2000000000000000111, 0.2062499999999999889, 0.2124999999999999944, 0.2187500000000000000, 0.2250000000000000056, 0.2312500000000000111, 0.2374999999999999889, 0.2437499999999999944, 0.2500000000000000000, 0.2562499999999999778, 0.2625000000000000111, 0.2687499999999999889, 0.2750000000000000222, 0.2812500000000000000, 0.2874999999999999778, 0.2937500000000000111, 0.2999999999999999889, 0.3062500000000000222, 0.3125000000000000000, 0.3187499999999999778, 0.3250000000000000111, 0.3312499999999999889, 0.3375000000000000222, 0.3437500000000000000, 0.3499999999999999778, 0.3562500000000000111, 0.3624999999999999889, 0.3687500000000000222, 0.3750000000000000000, 0.3812499999999999778, 0.3875000000000000111, 0.3937499999999999889, 0.4000000000000000222, 0.4062500000000000000, 0.4124999999999999778, 0.4187500000000000111, 0.4249999999999999889, 0.4312500000000000222, 0.4375000000000000000, 0.4437499999999999778, 0.4500000000000000111, 0.4562499999999999889, 0.4625000000000000222, 0.4687500000000000000, 0.4749999999999999778, 0.4812500000000000111, 0.4874999999999999889, 0.4937500000000000222, 0.5000000000000000000, 0.5062499999999999778, 0.5124999999999999556, 0.5187500000000000444, 0.5250000000000000222, 0.5312500000000000000, 0.5374999999999999778, 0.5437499999999999556, 0.5500000000000000444, 0.5562500000000000222, 0.5625000000000000000, 0.5687499999999999778, 0.5749999999999999556, 0.5812500000000000444, 0.5875000000000000222, 0.5937500000000000000, 0.5999999999999999778, 0.6062499999999999556, 0.6125000000000000444, 0.6187500000000000222, 0.6250000000000000000, 0.6312499999999999778, 0.6374999999999999556, 0.6437500000000000444, 0.6500000000000000222, 0.6562500000000000000, 0.6624999999999999778, 0.6687499999999999556, 0.6750000000000000444, 0.6812500000000000222, 0.6875000000000000000, 0.6937499999999999778, 0.6999999999999999556, 0.7062500000000000444, 0.7125000000000000222, 0.7187500000000000000, 0.7249999999999999778, 0.7312499999999999556, 0.7375000000000000444, 0.7437500000000000222, 0.7500000000000000000, 0.7562499999999999778, 0.7624999999999999556, 0.7687500000000000444, 0.7750000000000000222, 0.7812500000000000000, 0.7874999999999999778, 0.7937499999999999556, 0.8000000000000000444, 0.8062500000000000222, 0.8125000000000000000, 0.8187499999999999778, 0.8249999999999999556, 0.8312500000000000444, 0.8375000000000000222, 0.8437500000000000000, 0.8499999999999999778, 0.8562499999999999556, 0.8625000000000000444, 0.8687500000000000222, 0.8750000000000000000, 0.8812499999999999778, 0.8874999999999999556, 0.8937500000000000444, 0.9000000000000000222, 0.9062500000000000000, 0.9124999999999999778, 0.9187499999999999556, 0.9250000000000000444, 0.9312500000000000222, 0.9375000000000000000, 0.9437499999999999778, 0.9499999999999999556, 0.9562500000000000444, 0.9625000000000000222, 0.9687500000000000000 ),
 .UNSPECIFIED. ) 
 GEOMETRIC_REPRESENTATION_ITEM ( )  RATIONAL_B_SPLINE_SURFACE ( (
 ( 1.000000000000000000, 0.9510565162951535312, 1.000000000000000000, 0.9510565162951535312, 1.000000000000000000, 0.9510565162951535312, 1.000000000000000000, 0.9510565162951535312, 1.000000000000000000, 0.9510565162951535312, 1.000000000000000000, 0.9510565162951535312, 1.000000000000000000, 0.9510565162951535312, 1.000000000000000000, 0.9510565162951535312, 1.000000000000000000, 0.9510565162951535312, 1.000000000000000000, 0.9510565162951535312, 1.000000000000000000, 0.9510565162951535312, 1.000000000000000000, 0.9510565162951535312, 1.000000000000000000, 0.9510565162951535312, 1.000000000000000000, 0.9510565162951535312, 1.000000000000000000, 0.9510565162951535312, 1.000000000000000000, 0.9510565162951535312, 1.000000000000000000, 0.9510565162951535312, 1.000000000000000000, 0.9510565162951535312, 1.000000000000000000, 0.9510565162951535312, 1.000000000000000000, 0.9510565162951535312, 1.000000000000000000, 0.9510565162951535312, 1.000000000000000000, 0.9510565162951535312, 1.000000000000000000, 0.9510565162951535312, 1.000000000000000000, 0.9510565162951535312, 1.000000000000000000, 0.9510565162951535312, 1.000000000000000000, 0.9510565162951535312, 1.000000000000000000, 0.9510565162951535312, 1.000000000000000000, 0.9510565162951535312, 1.000000000000000000, 0.9510565162951535312, 1.000000000000000000, 0.9510565162951535312, 1.000000000000000000, 0.9510565162951535312, 1.000000000000000000, 0.9510565162951535312, 1.000000000000000000, 0.9510565162951535312, 1.000000000000000000, 0.9510565162951535312, 1.000000000000000000, 0.9510565162951535312, 1.000000000000000000, 0.9510565162951535312, 1.000000000000000000, 0.9510565162951535312, 1.000000000000000000, 0.9510565162951535312, 1.000000000000000000, 0.9510565162951535312, 1.000000000000000000, 0.9510565162951535312, 1.000000000000000000, 0.9510565162951535312, 1.000000000000000000, 0.9510565162951535312, 1.000000000000000000, 0.9510565162951535312, 1.000000000000000000, 0.9510565162951535312, 1.000000000000000000, 0.9510565162951535312, 1.000000000000000000, 0.9510565162951535312, 1.000000000000000000, 0.9510565162951535312, 1.000000000000000000, 0.9510565162951535312, 1.000000000000000000, 0.9510565162951535312, 1.000000000000000000, 0.9510565162951535312, 1.000000000000000000, 0.9510565162951535312, 1.000000000000000000, 0.9510565162951535312, 1.000000000000000000, 0.9510565162951535312, 1.000000000000000000, 0.9510565162951535312, 1.000000000000000000, 0.9510565162951535312, 1.000000000000000000, 0.9510565162951535312, 1.000000000000000000, 0.9510565162951535312, 1.000000000000000000, 0.9510565162951535312, 1.000000000000000000, 0.9510565162951535312, 1.000000000000000000, 0.9510565162951535312, 1.000000000000000000, 0.9510565162951535312, 1.000000000000000000, 0.9510565162951535312, 1.000000000000000000, 0.9510565162951535312, 1.000000000000000000, 0.9510565162951535312, 1.000000000000000000, 0.9510565162951535312, 1.000000000000000000, 0.9510565162951535312, 1.000000000000000000, 0.9510565162951535312, 1.000000000000000000, 0.9510565162951535312, 1.000000000000000000, 0.9510565162951535312, 1.000000000000000000, 0.9510565162951535312, 1.000000000000000000, 0.9510565162951535312, 1.000000000000000000, 0.9510565162951535312, 1.000000000000000000, 0.9510565162951535312, 1.000000000000000000, 0.9510565162951535312, 1.000000000000000000, 0.9510565162951535312, 1.000000000000000000, 0.9510565162951535312, 1.000000000000000000, 0.9510565162951535312, 1.000000000000000000, 0.9510565162951535312, 1.000000000000000000, 0.9510565162951535312, 1.000000000000000000, 0.9510565162951535312, 1.000000000000000000, 0.9510565162951535312, 1.000000000000000000, 0.9510565162951535312, 1.000000000000000000, 0.9510565162951535312, 1.000000000000000000, 0.9510565162951535312, 1.000000000000000000, 0.9510565162951535312, 1.000000000000000000, 0.9510565162951535312, 1.000000000000000000, 0.9510565162951535312, 1.000000000000000000, 0.9510565162951535312, 1.000000000000000000, 0.9510565162951535312, 1.000000000000000000, 0.9510565162951535312, 1.000000000000000000, 0.9510565162951535312, 1.000000000000000000, 0.9510565162951535312, 1.000000000000000000, 0.9510565162951535312, 1.000000000000000000, 0.9510565162951535312, 1.000000000000000000, 0.9510565162951535312, 1.000000000000000000, 0.9510565162951535312, 1.000000000000000000, 0.9510565162951535312, 1.000000000000000000, 0.9510565162951535312, 1.000000000000000000, 0.9510565162951535312, 1.000000000000000000, 0.9510565162951535312, 1.000000000000000000, 0.9510565162951535312, 1.000000000000000000, 0.9510565162951535312, 1.000000000000000000, 0.9510565162951535312, 1.000000000000000000, 0.9510565162951535312, 1.000000000000000000, 0.9510565162951535312, 1.000000000000000000, 0.9510565162951535312, 1.000000000000000000, 0.9510565162951535312, 1.000000000000000000, 0.9510565162951535312, 1.000000000000000000, 0.9510565162951535312, 1.000000000000000000, 0.9510565162951535312, 1.000000000000000000, 0.9510565162951535312, 1.000000000000000000, 0.9510565162951535312, 1.000000000000000000, 0.9510565162951535312, 1.000000000000000000, 0.9510565162951535312, 1.000000000000000000, 0.9510565162951535312, 1.000000000000000000, 0.9510565162951535312, 1.000000000000000000, 0.9510565162951535312, 1.000000000000000000, 0.9510565162951535312, 1.000000000000000000, 0.9510565162951535312, 1.000000000000000000, 0.9510565162951535312, 1.000000000000000000, 0.9510565162951535312, 1.000000000000000000, 0.9510565162951535312, 1.000000000000000000, 0.9510565162951535312, 1.000000000000000000, 0.9510565162951535312, 1.000000000000000000, 0.9510565162951535312, 1.000000000000000000, 0.9510565162951535312, 1.000000000000000000, 0.9510565162951535312, 1.000000000000000000, 0.9510565162951535312, 1.000000000000000000, 0.9510565162951535312, 1.000000000000000000, 0.9510565162951535312, 1.000000000000000000, 0.9510565162951535312, 1.000000000000000000, 0.9510565162951535312, 1.000000000000000000, 0.9510565162951535312, 1.000000000000000000, 0.9510565162951535312, 1.000000000000000000, 0.9510565162951535312, 1.000000000000000000, 0.9510565162951535312, 1.000000000000000000, 0.9510565162951535312, 1.000000000000000000, 0.9510565162951535312, 1.000000000000000000, 0.9510565162951535312, 1.000000000000000000, 0.9510565162951535312, 1.000000000000000000, 0.9510565162951535312, 1.000000000000000000, 0.9510565162951535312, 1.000000000000000000, 0.9510565162951535312, 1.000000000000000000, 0.9510565162951535312, 1.000000000000000000, 0.9510565162951535312, 1.000000000000000000, 0.9510565162951535312, 1.000000000000000000, 0.9510565162951535312, 1.000000000000000000, 0.9510565162951535312, 1.000000000000000000, 0.9510565162951535312, 1.000000000000000000, 0.9510565162951535312, 1.000000000000000000, 0.9510565162951535312, 1.000000000000000000, 0.9510565162951535312, 1.000000000000000000, 0.9510565162951535312, 1.000000000000000000, 0.9510565162951535312, 1.000000000000000000, 0.9510565162951535312, 1.000000000000000000),
 ( 0.3333333333333333703, 0.3170188387650512141, 0.3333333333333333703, 0.3170188387650512141, 0.3333333333333333703, 0.3170188387650512141, 0.3333333333333333703, 0.3170188387650512141, 0.3333333333333333703, 0.3170188387650512141, 0.3333333333333333703, 0.3170188387650512141, 0.3333333333333333703, 0.3170188387650512141, 0.3333333333333333703, 0.3170188387650512141, 0.3333333333333333703, 0.3170188387650512141, 0.3333333333333333703, 0.3170188387650512141, 0.3333333333333333703, 0.3170188387650512141, 0.3333333333333333703, 0.3170188387650512141, 0.3333333333333333703, 0.3170188387650512141, 0.3333333333333333703, 0.3170188387650512141, 0.3333333333333333703, 0.3170188387650512141, 0.3333333333333333703, 0.3170188387650512141, 0.3333333333333333703, 0.3170188387650512141, 0.3333333333333333703, 0.3170188387650512141, 0.3333333333333333703, 0.3170188387650512141, 0.3333333333333333703, 0.3170188387650512141, 0.3333333333333333703, 0.3170188387650512141, 0.3333333333333333703, 0.3170188387650512141, 0.3333333333333333703, 0.3170188387650512141, 0.3333333333333333703, 0.3170188387650512141, 0.3333333333333333703, 0.3170188387650512141, 0.3333333333333333703, 0.3170188387650512141, 0.3333333333333333703, 0.3170188387650512141, 0.3333333333333333703, 0.3170188387650512141, 0.3333333333333333703, 0.3170188387650512141, 0.3333333333333333703, 0.3170188387650512141, 0.3333333333333333703, 0.3170188387650512141, 0.3333333333333333703, 0.3170188387650512141, 0.3333333333333333703, 0.3170188387650512141, 0.3333333333333333703, 0.3170188387650512141, 0.3333333333333333703, 0.3170188387650512141, 0.3333333333333333703, 0.3170188387650512141, 0.3333333333333333703, 0.3170188387650512141, 0.3333333333333333703, 0.3170188387650512141, 0.3333333333333333703, 0.3170188387650512141, 0.3333333333333333703, 0.3170188387650512141, 0.3333333333333333703, 0.3170188387650512141, 0.3333333333333333703, 0.3170188387650512141, 0.3333333333333333703, 0.3170188387650512141, 0.3333333333333333703, 0.3170188387650512141, 0.3333333333333333703, 0.3170188387650512141, 0.3333333333333333703, 0.3170188387650512141, 0.3333333333333333703, 0.3170188387650512141, 0.3333333333333333703, 0.3170188387650512141, 0.3333333333333333703, 0.3170188387650512141, 0.3333333333333333703, 0.3170188387650512141, 0.3333333333333333703, 0.3170188387650512141, 0.3333333333333333703, 0.3170188387650512141, 0.3333333333333333703, 0.3170188387650512141, 0.3333333333333333703, 0.3170188387650512141, 0.3333333333333333703, 0.3170188387650512141, 0.3333333333333333703, 0.3170188387650512141, 0.3333333333333333703, 0.3170188387650512141, 0.3333333333333333703, 0.3170188387650512141, 0.3333333333333333703, 0.3170188387650512141, 0.3333333333333333703, 0.3170188387650512141, 0.3333333333333333703, 0.3170188387650512141, 0.3333333333333333703, 0.3170188387650512141, 0.3333333333333333703, 0.3170188387650512141, 0.3333333333333333703, 0.3170188387650512141, 0.3333333333333333703, 0.3170188387650512141, 0.3333333333333333703, 0.3170188387650512141, 0.3333333333333333703, 0.3170188387650512141, 0.3333333333333333703, 0.3170188387650512141, 0.3333333333333333703, 0.3170188387650512141, 0.3333333333333333703, 0.3170188387650512141, 0.3333333333333333703, 0.3170188387650512141, 0.3333333333333333703, 0.3170188387650512141, 0.3333333333333333703, 0.3170188387650512141, 0.3333333333333333703, 0.3170188387650512141, 0.3333333333333333703, 0.3170188387650512141, 0.3333333333333333703, 0.3170188387650512141, 0.3333333333333333703, 0.3170188387650512141, 0.3333333333333333703, 0.3170188387650512141, 0.3333333333333333703, 0.3170188387650512141, 0.3333333333333333703, 0.3170188387650512141, 0.3333333333333333703, 0.3170188387650512141, 0.3333333333333333703, 0.3170188387650512141, 0.3333333333333333703, 0.3170188387650512141, 0.3333333333333333703, 0.3170188387650512141, 0.3333333333333333703, 0.3170188387650512141, 0.3333333333333333703, 0.3170188387650512141, 0.3333333333333333703, 0.3170188387650512141, 0.3333333333333333703, 0.3170188387650512141, 0.3333333333333333703, 0.3170188387650512141, 0.3333333333333333703, 0.3170188387650512141, 0.3333333333333333703, 0.3170188387650512141, 0.3333333333333333703, 0.3170188387650512141, 0.3333333333333333703, 0.3170188387650512141, 0.3333333333333333703, 0.3170188387650512141, 0.3333333333333333703, 0.3170188387650512141, 0.3333333333333333703, 0.3170188387650512141, 0.3333333333333333703, 0.3170188387650512141, 0.3333333333333333703, 0.3170188387650512141, 0.3333333333333333703, 0.3170188387650512141, 0.3333333333333333703, 0.3170188387650512141, 0.3333333333333333703, 0.3170188387650512141, 0.3333333333333333703, 0.3170188387650512141, 0.3333333333333333703, 0.3170188387650512141, 0.3333333333333333703, 0.3170188387650512141, 0.3333333333333333703, 0.3170188387650512141, 0.3333333333333333703, 0.3170188387650512141, 0.3333333333333333703, 0.3170188387650512141, 0.3333333333333333703, 0.3170188387650512141, 0.3333333333333333703, 0.3170188387650512141, 0.3333333333333333703, 0.3170188387650512141, 0.3333333333333333703, 0.3170188387650512141, 0.3333333333333333703, 0.3170188387650512141, 0.3333333333333333703, 0.3170188387650512141, 0.3333333333333333703, 0.3170188387650512141, 0.3333333333333333703, 0.3170188387650512141, 0.3333333333333333703, 0.3170188387650512141, 0.3333333333333333703, 0.3170188387650512141, 0.3333333333333333703, 0.3170188387650512141, 0.3333333333333333703, 0.3170188387650512141, 0.3333333333333333703, 0.3170188387650512141, 0.3333333333333333703, 0.3170188387650512141, 0.3333333333333333703, 0.3170188387650512141, 0.3333333333333333703, 0.3170188387650512141, 0.3333333333333333703, 0.3170188387650512141, 0.3333333333333333703, 0.3170188387650512141, 0.3333333333333333703, 0.3170188387650512141, 0.3333333333333333703, 0.3170188387650512141, 0.3333333333333333703, 0.3170188387650512141, 0.3333333333333333703, 0.3170188387650512141, 0.3333333333333333703, 0.3170188387650512141, 0.3333333333333333703, 0.3170188387650512141, 0.3333333333333333703, 0.3170188387650512141, 0.3333333333333333703, 0.3170188387650512141, 0.3333333333333333703, 0.3170188387650512141, 0.3333333333333333703, 0.3170188387650512141, 0.3333333333333333703, 0.3170188387650512141, 0.3333333333333333703, 0.3170188387650512141, 0.3333333333333333703, 0.3170188387650512141, 0.3333333333333333703, 0.3170188387650512141, 0.3333333333333333703, 0.3170188387650512141, 0.3333333333333333703, 0.3170188387650512141, 0.3333333333333333703, 0.3170188387650512141, 0.3333333333333333703, 0.3170188387650512141, 0.3333333333333333703, 0.3170188387650512141, 0.3333333333333333703, 0.3170188387650512141, 0.3333333333333333703, 0.3170188387650512141, 0.3333333333333333703, 0.3170188387650512141, 0.3333333333333333703, 0.3170188387650512141, 0.3333333333333333703, 0.3170188387650512141, 0.3333333333333333703, 0.3170188387650512141, 0.3333333333333333703, 0.3170188387650512141, 0.3333333333333333703, 0.3170188387650512141, 0.3333333333333333703, 0.3170188387650512141, 0.3333333333333333703, 0.3170188387650512141, 0.3333333333333333703, 0.3170188387650512141, 0.3333333333333333703),
 ( 0.3333333333333333703, 0.3170188387650512141, 0.3333333333333333703, 0.3170188387650512141, 0.3333333333333333703, 0.3170188387650512141, 0.3333333333333333703, 0.3170188387650512141, 0.3333333333333333703, 0.3170188387650512141, 0.3333333333333333703, 0.3170188387650512141, 0.3333333333333333703, 0.3170188387650512141, 0.3333333333333333703, 0.3170188387650512141, 0.3333333333333333703, 0.3170188387650512141, 0.3333333333333333703, 0.3170188387650512141, 0.3333333333333333703, 0.3170188387650512141, 0.3333333333333333703, 0.3170188387650512141, 0.3333333333333333703, 0.3170188387650512141, 0.3333333333333333703, 0.3170188387650512141, 0.3333333333333333703, 0.3170188387650512141, 0.3333333333333333703, 0.3170188387650512141, 0.3333333333333333703, 0.3170188387650512141, 0.3333333333333333703, 0.3170188387650512141, 0.3333333333333333703, 0.3170188387650512141, 0.3333333333333333703, 0.3170188387650512141, 0.3333333333333333703, 0.3170188387650512141, 0.3333333333333333703, 0.3170188387650512141, 0.3333333333333333703, 0.3170188387650512141, 0.3333333333333333703, 0.3170188387650512141, 0.3333333333333333703, 0.3170188387650512141, 0.3333333333333333703, 0.3170188387650512141, 0.3333333333333333703, 0.3170188387650512141, 0.3333333333333333703, 0.3170188387650512141, 0.3333333333333333703, 0.3170188387650512141, 0.3333333333333333703, 0.3170188387650512141, 0.3333333333333333703, 0.3170188387650512141, 0.3333333333333333703, 0.3170188387650512141, 0.3333333333333333703, 0.3170188387650512141, 0.3333333333333333703, 0.3170188387650512141, 0.3333333333333333703, 0.3170188387650512141, 0.3333333333333333703, 0.3170188387650512141, 0.3333333333333333703, 0.3170188387650512141, 0.3333333333333333703, 0.3170188387650512141, 0.3333333333333333703, 0.3170188387650512141, 0.3333333333333333703, 0.3170188387650512141, 0.3333333333333333703, 0.3170188387650512141, 0.3333333333333333703, 0.3170188387650512141, 0.3333333333333333703, 0.3170188387650512141, 0.3333333333333333703, 0.3170188387650512141, 0.3333333333333333703, 0.3170188387650512141, 0.3333333333333333703, 0.3170188387650512141, 0.3333333333333333703, 0.3170188387650512141, 0.3333333333333333703, 0.3170188387650512141, 0.3333333333333333703, 0.3170188387650512141, 0.3333333333333333703, 0.3170188387650512141, 0.3333333333333333703, 0.3170188387650512141, 0.3333333333333333703, 0.3170188387650512141, 0.3333333333333333703, 0.3170188387650512141, 0.3333333333333333703, 0.3170188387650512141, 0.3333333333333333703, 0.3170188387650512141, 0.3333333333333333703, 0.3170188387650512141, 0.3333333333333333703, 0.3170188387650512141, 0.3333333333333333703, 0.3170188387650512141, 0.3333333333333333703, 0.3170188387650512141, 0.3333333333333333703, 0.3170188387650512141, 0.3333333333333333703, 0.3170188387650512141, 0.3333333333333333703, 0.3170188387650512141, 0.3333333333333333703, 0.3170188387650512141, 0.3333333333333333703, 0.3170188387650512141, 0.3333333333333333703, 0.3170188387650512141, 0.3333333333333333703, 0.3170188387650512141, 0.3333333333333333703, 0.3170188387650512141, 0.3333333333333333703, 0.3170188387650512141, 0.3333333333333333703, 0.3170188387650512141, 0.3333333333333333703, 0.3170188387650512141, 0.3333333333333333703, 0.3170188387650512141, 0.3333333333333333703, 0.3170188387650512141, 0.3333333333333333703, 0.3170188387650512141, 0.3333333333333333703, 0.3170188387650512141, 0.3333333333333333703, 0.3170188387650512141, 0.3333333333333333703, 0.3170188387650512141, 0.3333333333333333703, 0.3170188387650512141, 0.3333333333333333703, 0.3170188387650512141, 0.3333333333333333703, 0.3170188387650512141, 0.3333333333333333703, 0.3170188387650512141, 0.3333333333333333703, 0.3170188387650512141, 0.3333333333333333703, 0.3170188387650512141, 0.3333333333333333703, 0.3170188387650512141, 0.3333333333333333703, 0.3170188387650512141, 0.3333333333333333703, 0.3170188387650512141, 0.3333333333333333703, 0.3170188387650512141, 0.3333333333333333703, 0.3170188387650512141, 0.3333333333333333703, 0.3170188387650512141, 0.3333333333333333703, 0.3170188387650512141, 0.3333333333333333703, 0.3170188387650512141, 0.3333333333333333703, 0.3170188387650512141, 0.3333333333333333703, 0.3170188387650512141, 0.3333333333333333703, 0.3170188387650512141, 0.3333333333333333703, 0.3170188387650512141, 0.3333333333333333703, 0.3170188387650512141, 0.3333333333333333703, 0.3170188387650512141, 0.3333333333333333703, 0.3170188387650512141, 0.3333333333333333703, 0.3170188387650512141, 0.3333333333333333703, 0.3170188387650512141, 0.3333333333333333703, 0.3170188387650512141, 0.3333333333333333703, 0.3170188387650512141, 0.3333333333333333703, 0.3170188387650512141, 0.3333333333333333703, 0.3170188387650512141, 0.3333333333333333703, 0.3170188387650512141, 0.3333333333333333703, 0.3170188387650512141, 0.3333333333333333703, 0.3170188387650512141, 0.3333333333333333703, 0.3170188387650512141, 0.3333333333333333703, 0.3170188387650512141, 0.3333333333333333703, 0.3170188387650512141, 0.3333333333333333703, 0.3170188387650512141, 0.3333333333333333703, 0.3170188387650512141, 0.3333333333333333703, 0.3170188387650512141, 0.3333333333333333703, 0.3170188387650512141, 0.3333333333333333703, 0.3170188387650512141, 0.3333333333333333703, 0.3170188387650512141, 0.3333333333333333703, 0.3170188387650512141, 0.3333333333333333703, 0.3170188387650512141, 0.3333333333333333703, 0.3170188387650512141, 0.3333333333333333703, 0.3170188387650512141, 0.3333333333333333703, 0.3170188387650512141, 0.3333333333333333703, 0.3170188387650512141, 0.3333333333333333703, 0.3170188387650512141, 0.3333333333333333703, 0.3170188387650512141, 0.3333333333333333703, 0.3170188387650512141, 0.3333333333333333703, 0.3170188387650512141, 0.3333333333333333703, 0.3170188387650512141, 0.3333333333333333703, 0.3170188387650512141, 0.3333333333333333703, 0.3170188387650512141, 0.3333333333333333703, 0.3170188387650512141, 0.3333333333333333703, 0.3170188387650512141, 0.3333333333333333703, 0.3170188387650512141, 0.3333333333333333703, 0.3170188387650512141, 0.3333333333333333703, 0.3170188387650512141, 0.3333333333333333703, 0.3170188387650512141, 0.3333333333333333703, 0.3170188387650512141, 0.3333333333333333703, 0.3170188387650512141, 0.3333333333333333703, 0.3170188387650512141, 0.3333333333333333703, 0.3170188387650512141, 0.3333333333333333703, 0.3170188387650512141, 0.3333333333333333703, 0.3170188387650512141, 0.3333333333333333703, 0.3170188387650512141, 0.3333333333333333703, 0.3170188387650512141, 0.3333333333333333703, 0.3170188387650512141, 0.3333333333333333703, 0.3170188387650512141, 0.3333333333333333703, 0.3170188387650512141, 0.3333333333333333703, 0.3170188387650512141, 0.3333333333333333703, 0.3170188387650512141, 0.3333333333333333703, 0.3170188387650512141, 0.3333333333333333703, 0.3170188387650512141, 0.3333333333333333703, 0.3170188387650512141, 0.3333333333333333703, 0.3170188387650512141, 0.3333333333333333703, 0.3170188387650512141, 0.3333333333333333703, 0.3170188387650512141, 0.3333333333333333703, 0.3170188387650512141, 0.3333333333333333703, 0.3170188387650512141, 0.3333333333333333703),
 ( 1.000000000000000000, 0.9510565162951535312, 1.000000000000000000, 0.9510565162951535312, 1.000000000000000000, 0.9510565162951535312, 1.000000000000000000, 0.9510565162951535312, 1.000000000000000000, 0.9510565162951535312, 1.000000000000000000, 0.9510565162951535312, 1.000000000000000000, 0.9510565162951535312, 1.000000000000000000, 0.9510565162951535312, 1.000000000000000000, 0.9510565162951535312, 1.000000000000000000, 0.9510565162951535312, 1.000000000000000000, 0.9510565162951535312, 1.000000000000000000, 0.9510565162951535312, 1.000000000000000000, 0.9510565162951535312, 1.000000000000000000, 0.9510565162951535312, 1.000000000000000000, 0.9510565162951535312, 1.000000000000000000, 0.9510565162951535312, 1.000000000000000000, 0.9510565162951535312, 1.000000000000000000, 0.9510565162951535312, 1.000000000000000000, 0.9510565162951535312, 1.000000000000000000, 0.9510565162951535312, 1.000000000000000000, 0.9510565162951535312, 1.000000000000000000, 0.9510565162951535312, 1.000000000000000000, 0.9510565162951535312, 1.000000000000000000, 0.9510565162951535312, 1.000000000000000000, 0.9510565162951535312, 1.000000000000000000, 0.9510565162951535312, 1.000000000000000000, 0.9510565162951535312, 1.000000000000000000, 0.9510565162951535312, 1.000000000000000000, 0.9510565162951535312, 1.000000000000000000, 0.9510565162951535312, 1.000000000000000000, 0.9510565162951535312, 1.000000000000000000, 0.9510565162951535312, 1.000000000000000000, 0.9510565162951535312, 1.000000000000000000, 0.9510565162951535312, 1.000000000000000000, 0.9510565162951535312, 1.000000000000000000, 0.9510565162951535312, 1.000000000000000000, 0.9510565162951535312, 1.000000000000000000, 0.9510565162951535312, 1.000000000000000000, 0.9510565162951535312, 1.000000000000000000, 0.9510565162951535312, 1.000000000000000000, 0.9510565162951535312, 1.000000000000000000, 0.9510565162951535312, 1.000000000000000000, 0.9510565162951535312, 1.000000000000000000, 0.9510565162951535312, 1.000000000000000000, 0.9510565162951535312, 1.000000000000000000, 0.9510565162951535312, 1.000000000000000000, 0.9510565162951535312, 1.000000000000000000, 0.9510565162951535312, 1.000000000000000000, 0.9510565162951535312, 1.000000000000000000, 0.9510565162951535312, 1.000000000000000000, 0.9510565162951535312, 1.000000000000000000, 0.9510565162951535312, 1.000000000000000000, 0.9510565162951535312, 1.000000000000000000, 0.9510565162951535312, 1.000000000000000000, 0.9510565162951535312, 1.000000000000000000, 0.9510565162951535312, 1.000000000000000000, 0.9510565162951535312, 1.000000000000000000, 0.9510565162951535312, 1.000000000000000000, 0.9510565162951535312, 1.000000000000000000, 0.9510565162951535312, 1.000000000000000000, 0.9510565162951535312, 1.000000000000000000, 0.9510565162951535312, 1.000000000000000000, 0.9510565162951535312, 1.000000000000000000, 0.9510565162951535312, 1.000000000000000000, 0.9510565162951535312, 1.000000000000000000, 0.9510565162951535312, 1.000000000000000000, 0.9510565162951535312, 1.000000000000000000, 0.9510565162951535312, 1.000000000000000000, 0.9510565162951535312, 1.000000000000000000, 0.9510565162951535312, 1.000000000000000000, 0.9510565162951535312, 1.000000000000000000, 0.9510565162951535312, 1.000000000000000000, 0.9510565162951535312, 1.000000000000000000, 0.9510565162951535312, 1.000000000000000000, 0.9510565162951535312, 1.000000000000000000, 0.9510565162951535312, 1.000000000000000000, 0.9510565162951535312, 1.000000000000000000, 0.9510565162951535312, 1.000000000000000000, 0.9510565162951535312, 1.000000000000000000, 0.9510565162951535312, 1.000000000000000000, 0.9510565162951535312, 1.000000000000000000, 0.9510565162951535312, 1.000000000000000000, 0.9510565162951535312, 1.000000000000000000, 0.9510565162951535312, 1.000000000000000000, 0.9510565162951535312, 1.000000000000000000, 0.9510565162951535312, 1.000000000000000000, 0.9510565162951535312, 1.000000000000000000, 0.9510565162951535312, 1.000000000000000000, 0.9510565162951535312, 1.000000000000000000, 0.9510565162951535312, 1.000000000000000000, 0.9510565162951535312, 1.000000000000000000, 0.9510565162951535312, 1.000000000000000000, 0.9510565162951535312, 1.000000000000000000, 0.9510565162951535312, 1.000000000000000000, 0.9510565162951535312, 1.000000000000000000, 0.9510565162951535312, 1.000000000000000000, 0.9510565162951535312, 1.000000000000000000, 0.9510565162951535312, 1.000000000000000000, 0.9510565162951535312, 1.000000000000000000, 0.9510565162951535312, 1.000000000000000000, 0.9510565162951535312, 1.000000000000000000, 0.9510565162951535312, 1.000000000000000000, 0.9510565162951535312, 1.000000000000000000, 0.9510565162951535312, 1.000000000000000000, 0.9510565162951535312, 1.000000000000000000, 0.9510565162951535312, 1.000000000000000000, 0.9510565162951535312, 1.000000000000000000, 0.9510565162951535312, 1.000000000000000000, 0.9510565162951535312, 1.000000000000000000, 0.9510565162951535312, 1.000000000000000000, 0.9510565162951535312, 1.000000000000000000, 0.9510565162951535312, 1.000000000000000000, 0.9510565162951535312, 1.000000000000000000, 0.9510565162951535312, 1.000000000000000000, 0.9510565162951535312, 1.000000000000000000, 0.9510565162951535312, 1.000000000000000000, 0.9510565162951535312, 1.000000000000000000, 0.9510565162951535312, 1.000000000000000000, 0.9510565162951535312, 1.000000000000000000, 0.9510565162951535312, 1.000000000000000000, 0.9510565162951535312, 1.000000000000000000, 0.9510565162951535312, 1.000000000000000000, 0.9510565162951535312, 1.000000000000000000, 0.9510565162951535312, 1.000000000000000000, 0.9510565162951535312, 1.000000000000000000, 0.9510565162951535312, 1.000000000000000000, 0.9510565162951535312, 1.000000000000000000, 0.9510565162951535312, 1.000000000000000000, 0.9510565162951535312, 1.000000000000000000, 0.9510565162951535312, 1.000000000000000000, 0.9510565162951535312, 1.000000000000000000, 0.9510565162951535312, 1.000000000000000000, 0.9510565162951535312, 1.000000000000000000, 0.9510565162951535312, 1.000000000000000000, 0.9510565162951535312, 1.000000000000000000, 0.9510565162951535312, 1.000000000000000000, 0.9510565162951535312, 1.000000000000000000, 0.9510565162951535312, 1.000000000000000000, 0.9510565162951535312, 1.000000000000000000, 0.9510565162951535312, 1.000000000000000000, 0.9510565162951535312, 1.000000000000000000, 0.9510565162951535312, 1.000000000000000000, 0.9510565162951535312, 1.000000000000000000, 0.9510565162951535312, 1.000000000000000000, 0.9510565162951535312, 1.000000000000000000, 0.9510565162951535312, 1.000000000000000000, 0.9510565162951535312, 1.000000000000000000, 0.9510565162951535312, 1.000000000000000000, 0.9510565162951535312, 1.000000000000000000, 0.9510565162951535312, 1.000000000000000000, 0.9510565162951535312, 1.000000000000000000, 0.9510565162951535312, 1.000000000000000000, 0.9510565162951535312, 1.000000000000000000, 0.9510565162951535312, 1.000000000000000000, 0.9510565162951535312, 1.000000000000000000),
 ( 0.3333333333333333703, 0.3170188387650512141, 0.3333333333333333703, 0.3170188387650512141, 0.3333333333333333703, 0.3170188387650512141, 0.3333333333333333703, 0.3170188387650512141, 0.3333333333333333703, 0.3170188387650512141, 0.3333333333333333703, 0.3170188387650512141, 0.3333333333333333703, 0.3170188387650512141, 0.3333333333333333703, 0.3170188387650512141, 0.3333333333333333703, 0.3170188387650512141, 0.3333333333333333703, 0.3170188387650512141, 0.3333333333333333703, 0.3170188387650512141, 0.3333333333333333703, 0.3170188387650512141, 0.3333333333333333703, 0.3170188387650512141, 0.3333333333333333703, 0.3170188387650512141, 0.3333333333333333703, 0.3170188387650512141, 0.3333333333333333703, 0.3170188387650512141, 0.3333333333333333703, 0.3170188387650512141, 0.3333333333333333703, 0.3170188387650512141, 0.3333333333333333703, 0.3170188387650512141, 0.3333333333333333703, 0.3170188387650512141, 0.3333333333333333703, 0.3170188387650512141, 0.3333333333333333703, 0.3170188387650512141, 0.3333333333333333703, 0.3170188387650512141, 0.3333333333333333703, 0.3170188387650512141, 0.3333333333333333703, 0.3170188387650512141, 0.3333333333333333703, 0.3170188387650512141, 0.3333333333333333703, 0.3170188387650512141, 0.3333333333333333703, 0.3170188387650512141, 0.3333333333333333703, 0.3170188387650512141, 0.3333333333333333703, 0.3170188387650512141, 0.3333333333333333703, 0.3170188387650512141, 0.3333333333333333703, 0.3170188387650512141, 0.3333333333333333703, 0.3170188387650512141, 0.3333333333333333703, 0.3170188387650512141, 0.3333333333333333703, 0.3170188387650512141, 0.3333333333333333703, 0.3170188387650512141, 0.3333333333333333703, 0.3170188387650512141, 0.3333333333333333703, 0.3170188387650512141, 0.3333333333333333703, 0.3170188387650512141, 0.3333333333333333703, 0.3170188387650512141, 0.3333333333333333703, 0.3170188387650512141, 0.3333333333333333703, 0.3170188387650512141, 0.3333333333333333703, 0.3170188387650512141, 0.3333333333333333703, 0.3170188387650512141, 0.3333333333333333703, 0.3170188387650512141, 0.3333333333333333703, 0.3170188387650512141, 0.3333333333333333703, 0.3170188387650512141, 0.3333333333333333703, 0.3170188387650512141, 0.3333333333333333703, 0.3170188387650512141, 0.3333333333333333703, 0.3170188387650512141, 0.3333333333333333703, 0.3170188387650512141, 0.3333333333333333703, 0.3170188387650512141, 0.3333333333333333703, 0.3170188387650512141, 0.3333333333333333703, 0.3170188387650512141, 0.3333333333333333703, 0.3170188387650512141, 0.3333333333333333703, 0.3170188387650512141, 0.3333333333333333703, 0.3170188387650512141, 0.3333333333333333703, 0.3170188387650512141, 0.3333333333333333703, 0.3170188387650512141, 0.3333333333333333703, 0.3170188387650512141, 0.3333333333333333703, 0.3170188387650512141, 0.3333333333333333703, 0.3170188387650512141, 0.3333333333333333703, 0.3170188387650512141, 0.3333333333333333703, 0.3170188387650512141, 0.3333333333333333703, 0.3170188387650512141, 0.3333333333333333703, 0.3170188387650512141, 0.3333333333333333703, 0.3170188387650512141, 0.3333333333333333703, 0.3170188387650512141, 0.3333333333333333703, 0.3170188387650512141, 0.3333333333333333703, 0.3170188387650512141, 0.3333333333333333703, 0.3170188387650512141, 0.3333333333333333703, 0.3170188387650512141, 0.3333333333333333703, 0.3170188387650512141, 0.3333333333333333703, 0.3170188387650512141, 0.3333333333333333703, 0.3170188387650512141, 0.3333333333333333703, 0.3170188387650512141, 0.3333333333333333703, 0.3170188387650512141, 0.3333333333333333703, 0.3170188387650512141, 0.3333333333333333703, 0.3170188387650512141, 0.3333333333333333703, 0.3170188387650512141, 0.3333333333333333703, 0.3170188387650512141, 0.3333333333333333703, 0.3170188387650512141, 0.3333333333333333703, 0.3170188387650512141, 0.3333333333333333703, 0.3170188387650512141, 0.3333333333333333703, 0.3170188387650512141, 0.3333333333333333703, 0.3170188387650512141, 0.3333333333333333703, 0.3170188387650512141, 0.3333333333333333703, 0.3170188387650512141, 0.3333333333333333703, 0.3170188387650512141, 0.3333333333333333703, 0.3170188387650512141, 0.3333333333333333703, 0.3170188387650512141, 0.3333333333333333703, 0.3170188387650512141, 0.3333333333333333703, 0.3170188387650512141, 0.3333333333333333703, 0.3170188387650512141, 0.3333333333333333703, 0.3170188387650512141, 0.3333333333333333703, 0.3170188387650512141, 0.3333333333333333703, 0.3170188387650512141, 0.3333333333333333703, 0.3170188387650512141, 0.3333333333333333703, 0.3170188387650512141, 0.3333333333333333703, 0.3170188387650512141, 0.3333333333333333703, 0.3170188387650512141, 0.3333333333333333703, 0.3170188387650512141, 0.3333333333333333703, 0.3170188387650512141, 0.3333333333333333703, 0.3170188387650512141, 0.3333333333333333703, 0.3170188387650512141, 0.3333333333333333703, 0.3170188387650512141, 0.3333333333333333703, 0.3170188387650512141, 0.3333333333333333703, 0.3170188387650512141, 0.3333333333333333703, 0.3170188387650512141, 0.3333333333333333703, 0.3170188387650512141, 0.3333333333333333703, 0.3170188387650512141, 0.3333333333333333703, 0.3170188387650512141, 0.3333333333333333703, 0.3170188387650512141, 0.3333333333333333703, 0.3170188387650512141, 0.3333333333333333703, 0.3170188387650512141, 0.3333333333333333703, 0.3170188387650512141, 0.3333333333333333703, 0.3170188387650512141, 0.3333333333333333703, 0.3170188387650512141, 0.3333333333333333703, 0.3170188387650512141, 0.3333333333333333703, 0.3170188387650512141, 0.3333333333333333703, 0.3170188387650512141, 0.3333333333333333703, 0.3170188387650512141, 0.3333333333333333703, 0.3170188387650512141, 0.3333333333333333703, 0.3170188387650512141, 0.3333333333333333703, 0.3170188387650512141, 0.3333333333333333703, 0.3170188387650512141, 0.3333333333333333703, 0.3170188387650512141, 0.3333333333333333703, 0.3170188387650512141, 0.3333333333333333703, 0.3170188387650512141, 0.3333333333333333703, 0.3170188387650512141, 0.3333333333333333703, 0.3170188387650512141, 0.3333333333333333703, 0.3170188387650512141, 0.3333333333333333703, 0.3170188387650512141, 0.3333333333333333703, 0.3170188387650512141, 0.3333333333333333703, 0.3170188387650512141, 0.3333333333333333703, 0.3170188387650512141, 0.3333333333333333703, 0.3170188387650512141, 0.3333333333333333703, 0.3170188387650512141, 0.3333333333333333703, 0.3170188387650512141, 0.3333333333333333703, 0.3170188387650512141, 0.3333333333333333703, 0.3170188387650512141, 0.3333333333333333703, 0.3170188387650512141, 0.3333333333333333703, 0.3170188387650512141, 0.3333333333333333703, 0.3170188387650512141, 0.3333333333333333703, 0.3170188387650512141, 0.3333333333333333703, 0.3170188387650512141, 0.3333333333333333703, 0.3170188387650512141, 0.3333333333333333703, 0.3170188387650512141, 0.3333333333333333703, 0.3170188387650512141, 0.3333333333333333703, 0.3170188387650512141, 0.3333333333333333703, 0.3170188387650512141, 0.3333333333333333703, 0.3170188387650512141, 0.3333333333333333703, 0.3170188387650512141, 0.3333333333333333703, 0.3170188387650512141, 0.3333333333333333703, 0.3170188387650512141, 0.3333333333333333703),
 ( 0.3333333333333333703, 0.3170188387650512141, 0.3333333333333333703, 0.3170188387650512141, 0.3333333333333333703, 0.3170188387650512141, 0.3333333333333333703, 0.3170188387650512141, 0.3333333333333333703, 0.3170188387650512141, 0.3333333333333333703, 0.3170188387650512141, 0.3333333333333333703, 0.3170188387650512141, 0.3333333333333333703, 0.3170188387650512141, 0.3333333333333333703, 0.3170188387650512141, 0.3333333333333333703, 0.3170188387650512141, 0.3333333333333333703, 0.3170188387650512141, 0.3333333333333333703, 0.3170188387650512141, 0.3333333333333333703, 0.3170188387650512141, 0.3333333333333333703, 0.3170188387650512141, 0.3333333333333333703, 0.3170188387650512141, 0.3333333333333333703, 0.3170188387650512141, 0.3333333333333333703, 0.3170188387650512141, 0.3333333333333333703, 0.3170188387650512141, 0.3333333333333333703, 0.3170188387650512141, 0.3333333333333333703, 0.3170188387650512141, 0.3333333333333333703, 0.3170188387650512141, 0.3333333333333333703, 0.3170188387650512141, 0.3333333333333333703, 0.3170188387650512141, 0.3333333333333333703, 0.3170188387650512141, 0.3333333333333333703, 0.3170188387650512141, 0.3333333333333333703, 0.3170188387650512141, 0.3333333333333333703, 0.3170188387650512141, 0.3333333333333333703, 0.3170188387650512141, 0.3333333333333333703, 0.3170188387650512141, 0.3333333333333333703, 0.3170188387650512141, 0.3333333333333333703, 0.3170188387650512141, 0.3333333333333333703, 0.3170188387650512141, 0.3333333333333333703, 0.3170188387650512141, 0.3333333333333333703, 0.3170188387650512141, 0.3333333333333333703, 0.3170188387650512141, 0.3333333333333333703, 0.3170188387650512141, 0.3333333333333333703, 0.3170188387650512141, 0.3333333333333333703, 0.3170188387650512141, 0.3333333333333333703, 0.3170188387650512141, 0.3333333333333333703, 0.3170188387650512141, 0.3333333333333333703, 0.3170188387650512141, 0.3333333333333333703, 0.3170188387650512141, 0.3333333333333333703, 0.3170188387650512141, 0.3333333333333333703, 0.3170188387650512141, 0.3333333333333333703, 0.3170188387650512141, 0.3333333333333333703, 0.3170188387650512141, 0.3333333333333333703, 0.3170188387650512141, 0.3333333333333333703, 0.3170188387650512141, 0.3333333333333333703, 0.3170188387650512141, 0.3333333333333333703, 0.3170188387650512141, 0.3333333333333333703, 0.3170188387650512141, 0.3333333333333333703, 0.3170188387650512141, 0.3333333333333333703, 0.3170188387650512141, 0.3333333333333333703, 0.3170188387650512141, 0.3333333333333333703, 0.3170188387650512141, 0.3333333333333333703, 0.3170188387650512141, 0.3333333333333333703, 0.3170188387650512141, 0.3333333333333333703, 0.3170188387650512141, 0.3333333333333333703, 0.3170188387650512141, 0.3333333333333333703, 0.3170188387650512141, 0.3333333333333333703, 0.3170188387650512141, 0.3333333333333333703, 0.3170188387650512141, 0.3333333333333333703, 0.3170188387650512141, 0.3333333333333333703, 0.3170188387650512141, 0.3333333333333333703, 0.3170188387650512141, 0.3333333333333333703, 0.3170188387650512141, 0.3333333333333333703, 0.3170188387650512141, 0.3333333333333333703, 0.3170188387650512141, 0.3333333333333333703, 0.3170188387650512141, 0.3333333333333333703, 0.3170188387650512141, 0.3333333333333333703, 0.3170188387650512141, 0.3333333333333333703, 0.3170188387650512141, 0.3333333333333333703, 0.3170188387650512141, 0.3333333333333333703, 0.3170188387650512141, 0.3333333333333333703, 0.3170188387650512141, 0.3333333333333333703, 0.3170188387650512141, 0.3333333333333333703, 0.3170188387650512141, 0.3333333333333333703, 0.3170188387650512141, 0.3333333333333333703, 0.3170188387650512141, 0.3333333333333333703, 0.3170188387650512141, 0.3333333333333333703, 0.3170188387650512141, 0.3333333333333333703, 0.3170188387650512141, 0.3333333333333333703, 0.3170188387650512141, 0.3333333333333333703, 0.3170188387650512141, 0.3333333333333333703, 0.3170188387650512141, 0.3333333333333333703, 0.3170188387650512141, 0.3333333333333333703, 0.3170188387650512141, 0.3333333333333333703, 0.3170188387650512141, 0.3333333333333333703, 0.3170188387650512141, 0.3333333333333333703, 0.3170188387650512141, 0.3333333333333333703, 0.3170188387650512141, 0.3333333333333333703, 0.3170188387650512141, 0.3333333333333333703, 0.3170188387650512141, 0.3333333333333333703, 0.3170188387650512141, 0.3333333333333333703, 0.3170188387650512141, 0.3333333333333333703, 0.3170188387650512141, 0.3333333333333333703, 0.3170188387650512141, 0.3333333333333333703, 0.3170188387650512141, 0.3333333333333333703, 0.3170188387650512141, 0.3333333333333333703, 0.3170188387650512141, 0.3333333333333333703, 0.3170188387650512141, 0.3333333333333333703, 0.3170188387650512141, 0.3333333333333333703, 0.3170188387650512141, 0.3333333333333333703, 0.3170188387650512141, 0.3333333333333333703, 0.3170188387650512141, 0.3333333333333333703, 0.3170188387650512141, 0.3333333333333333703, 0.3170188387650512141, 0.3333333333333333703, 0.3170188387650512141, 0.3333333333333333703, 0.3170188387650512141, 0.3333333333333333703, 0.3170188387650512141, 0.3333333333333333703, 0.3170188387650512141, 0.3333333333333333703, 0.3170188387650512141, 0.3333333333333333703, 0.3170188387650512141, 0.3333333333333333703, 0.3170188387650512141, 0.3333333333333333703, 0.3170188387650512141, 0.3333333333333333703, 0.3170188387650512141, 0.3333333333333333703, 0.3170188387650512141, 0.3333333333333333703, 0.3170188387650512141, 0.3333333333333333703, 0.3170188387650512141, 0.3333333333333333703, 0.3170188387650512141, 0.3333333333333333703, 0.3170188387650512141, 0.3333333333333333703, 0.3170188387650512141, 0.3333333333333333703, 0.3170188387650512141, 0.3333333333333333703, 0.3170188387650512141, 0.3333333333333333703, 0.3170188387650512141, 0.3333333333333333703, 0.3170188387650512141, 0.3333333333333333703, 0.3170188387650512141, 0.3333333333333333703, 0.3170188387650512141, 0.3333333333333333703, 0.3170188387650512141, 0.3333333333333333703, 0.3170188387650512141, 0.3333333333333333703, 0.3170188387650512141, 0.3333333333333333703, 0.3170188387650512141, 0.3333333333333333703, 0.3170188387650512141, 0.3333333333333333703, 0.3170188387650512141, 0.3333333333333333703, 0.3170188387650512141, 0.3333333333333333703, 0.3170188387650512141, 0.3333333333333333703, 0.3170188387650512141, 0.3333333333333333703, 0.3170188387650512141, 0.3333333333333333703, 0.3170188387650512141, 0.3333333333333333703, 0.3170188387650512141, 0.3333333333333333703, 0.3170188387650512141, 0.3333333333333333703, 0.3170188387650512141, 0.3333333333333333703, 0.3170188387650512141, 0.3333333333333333703, 0.3170188387650512141, 0.3333333333333333703, 0.3170188387650512141, 0.3333333333333333703, 0.3170188387650512141, 0.3333333333333333703, 0.3170188387650512141, 0.3333333333333333703, 0.3170188387650512141, 0.3333333333333333703, 0.3170188387650512141, 0.3333333333333333703, 0.3170188387650512141, 0.3333333333333333703, 0.3170188387650512141, 0.3333333333333333703, 0.3170188387650512141, 0.3333333333333333703, 0.3170188387650512141, 0.3333333333333333703, 0.3170188387650512141, 0.3333333333333333703, 0.3170188387650512141, 0.3333333333333333703),
 ( 1.000000000000000000, 0.9510565162951535312, 1.000000000000000000, 0.9510565162951535312, 1.000000000000000000, 0.9510565162951535312, 1.000000000000000000, 0.9510565162951535312, 1.000000000000000000, 0.9510565162951535312, 1.000000000000000000, 0.9510565162951535312, 1.000000000000000000, 0.9510565162951535312, 1.000000000000000000, 0.9510565162951535312, 1.000000000000000000, 0.9510565162951535312, 1.000000000000000000, 0.9510565162951535312, 1.000000000000000000, 0.9510565162951535312, 1.000000000000000000, 0.9510565162951535312, 1.000000000000000000, 0.9510565162951535312, 1.000000000000000000, 0.9510565162951535312, 1.000000000000000000, 0.9510565162951535312, 1.000000000000000000, 0.9510565162951535312, 1.000000000000000000, 0.9510565162951535312, 1.000000000000000000, 0.9510565162951535312, 1.000000000000000000, 0.9510565162951535312, 1.000000000000000000, 0.9510565162951535312, 1.000000000000000000, 0.9510565162951535312, 1.000000000000000000, 0.9510565162951535312, 1.000000000000000000, 0.9510565162951535312, 1.000000000000000000, 0.9510565162951535312, 1.000000000000000000, 0.9510565162951535312, 1.000000000000000000, 0.9510565162951535312, 1.000000000000000000, 0.9510565162951535312, 1.000000000000000000, 0.9510565162951535312, 1.000000000000000000, 0.9510565162951535312, 1.000000000000000000, 0.9510565162951535312, 1.000000000000000000, 0.9510565162951535312, 1.000000000000000000, 0.9510565162951535312, 1.000000000000000000, 0.9510565162951535312, 1.000000000000000000, 0.9510565162951535312, 1.000000000000000000, 0.9510565162951535312, 1.000000000000000000, 0.9510565162951535312, 1.000000000000000000, 0.9510565162951535312, 1.000000000000000000, 0.9510565162951535312, 1.000000000000000000, 0.9510565162951535312, 1.000000000000000000, 0.9510565162951535312, 1.000000000000000000, 0.9510565162951535312, 1.000000000000000000, 0.9510565162951535312, 1.000000000000000000, 0.9510565162951535312, 1.000000000000000000, 0.9510565162951535312, 1.000000000000000000, 0.9510565162951535312, 1.000000000000000000, 0.9510565162951535312, 1.000000000000000000, 0.9510565162951535312, 1.000000000000000000, 0.9510565162951535312, 1.000000000000000000, 0.9510565162951535312, 1.000000000000000000, 0.9510565162951535312, 1.000000000000000000, 0.9510565162951535312, 1.000000000000000000, 0.9510565162951535312, 1.000000000000000000, 0.9510565162951535312, 1.000000000000000000, 0.9510565162951535312, 1.000000000000000000, 0.9510565162951535312, 1.000000000000000000, 0.9510565162951535312, 1.000000000000000000, 0.9510565162951535312, 1.000000000000000000, 0.9510565162951535312, 1.000000000000000000, 0.9510565162951535312, 1.000000000000000000, 0.9510565162951535312, 1.000000000000000000, 0.9510565162951535312, 1.000000000000000000, 0.9510565162951535312, 1.000000000000000000, 0.9510565162951535312, 1.000000000000000000, 0.9510565162951535312, 1.000000000000000000, 0.9510565162951535312, 1.000000000000000000, 0.9510565162951535312, 1.000000000000000000, 0.9510565162951535312, 1.000000000000000000, 0.9510565162951535312, 1.000000000000000000, 0.9510565162951535312, 1.000000000000000000, 0.9510565162951535312, 1.000000000000000000, 0.9510565162951535312, 1.000000000000000000, 0.9510565162951535312, 1.000000000000000000, 0.9510565162951535312, 1.000000000000000000, 0.9510565162951535312, 1.000000000000000000, 0.9510565162951535312, 1.000000000000000000, 0.9510565162951535312, 1.000000000000000000, 0.9510565162951535312, 1.000000000000000000, 0.9510565162951535312, 1.000000000000000000, 0.9510565162951535312, 1.000000000000000000, 0.9510565162951535312, 1.000000000000000000, 0.9510565162951535312, 1.000000000000000000, 0.9510565162951535312, 1.000000000000000000, 0.9510565162951535312, 1.000000000000000000, 0.9510565162951535312, 1.000000000000000000, 0.9510565162951535312, 1.000000000000000000, 0.9510565162951535312, 1.000000000000000000, 0.9510565162951535312, 1.000000000000000000, 0.9510565162951535312, 1.000000000000000000, 0.9510565162951535312, 1.000000000000000000, 0.9510565162951535312, 1.000000000000000000, 0.9510565162951535312, 1.000000000000000000, 0.9510565162951535312, 1.000000000000000000, 0.9510565162951535312, 1.000000000000000000, 0.9510565162951535312, 1.000000000000000000, 0.9510565162951535312, 1.000000000000000000, 0.9510565162951535312, 1.000000000000000000, 0.9510565162951535312, 1.000000000000000000, 0.9510565162951535312, 1.000000000000000000, 0.9510565162951535312, 1.000000000000000000, 0.9510565162951535312, 1.000000000000000000, 0.9510565162951535312, 1.000000000000000000, 0.9510565162951535312, 1.000000000000000000, 0.9510565162951535312, 1.000000000000000000, 0.9510565162951535312, 1.000000000000000000, 0.9510565162951535312, 1.000000000000000000, 0.9510565162951535312, 1.000000000000000000, 0.9510565162951535312, 1.000000000000000000, 0.9510565162951535312, 1.000000000000000000, 0.9510565162951535312, 1.000000000000000000, 0.9510565162951535312, 1.000000000000000000, 0.9510565162951535312, 1.000000000000000000, 0.9510565162951535312, 1.000000000000000000, 0.9510565162951535312, 1.000000000000000000, 0.9510565162951535312, 1.000000000000000000, 0.9510565162951535312, 1.000000000000000000, 0.9510565162951535312, 1.000000000000000000, 0.9510565162951535312, 1.000000000000000000, 0.9510565162951535312, 1.000000000000000000, 0.9510565162951535312, 1.000000000000000000, 0.9510565162951535312, 1.000000000000000000, 0.9510565162951535312, 1.000000000000000000, 0.9510565162951535312, 1.000000000000000000, 0.9510565162951535312, 1.000000000000000000, 0.9510565162951535312, 1.000000000000000000, 0.9510565162951535312, 1.000000000000000000, 0.9510565162951535312, 1.000000000000000000, 0.9510565162951535312, 1.000000000000000000, 0.9510565162951535312, 1.000000000000000000, 0.9510565162951535312, 1.000000000000000000, 0.9510565162951535312, 1.000000000000000000, 0.9510565162951535312, 1.000000000000000000, 0.9510565162951535312, 1.000000000000000000, 0.9510565162951535312, 1.000000000000000000, 0.9510565162951535312, 1.000000000000000000, 0.9510565162951535312, 1.000000000000000000, 0.9510565162951535312, 1.000000000000000000, 0.9510565162951535312, 1.000000000000000000, 0.9510565162951535312, 1.000000000000000000, 0.9510565162951535312, 1.000000000000000000, 0.9510565162951535312, 1.000000000000000000, 0.9510565162951535312, 1.000000000000000000, 0.9510565162951535312, 1.000000000000000000, 0.9510565162951535312, 1.000000000000000000, 0.9510565162951535312, 1.000000000000000000, 0.9510565162951535312, 1.000000000000000000, 0.9510565162951535312, 1.000000000000000000, 0.9510565162951535312, 1.000000000000000000, 0.9510565162951535312, 1.000000000000000000, 0.9510565162951535312, 1.000000000000000000, 0.9510565162951535312, 1.000000000000000000, 0.9510565162951535312, 1.000000000000000000, 0.9510565162951535312, 1.000000000000000000, 0.9510565162951535312, 1.000000000000000000, 0.9510565162951535312, 1.000000000000000000, 0.9510565162951535312, 1.000000000000000000) ) ) 
 REPRESENTATION_ITEM ( '' )  SURFACE ( )  );
#19142 = ORIENTED_EDGE ( 'NONE', *, *, #14473, .T. ) ;
#19143 = LINE ( 'NONE', #1479, #15163 ) ;
#19144 = FACE_OUTER_BOUND ( 'NONE', #14640, .T. ) ;
#19145 = DIRECTION ( 'NONE',  ( -1.000000000000000000, -2.602085213965208275E-15, 0.000000000000000000 ) ) ;
#19146 = ORIENTED_EDGE ( 'NONE', *, *, #6443, .T. ) ;
#19147 = FACE_OUTER_BOUND ( 'NONE', #22601, .T. ) ;
#19148 = ORIENTED_EDGE ( 'NONE', *, *, #11549, .F. ) ;
#19149 = ORIENTED_EDGE ( 'NONE', *, *, #23909, .F. ) ;
#19150 = CARTESIAN_POINT ( 'NONE',  ( 43.52384487926482848, 3.236615080648331144, 6.150472170364783331 ) ) ;
#19151 = DIRECTION ( 'NONE',  ( 1.000000000000000000, 1.734723475976799945E-16, -1.734723475976814737E-16 ) ) ;
#19152 = CARTESIAN_POINT ( 'NONE',  ( 37.12184278917507640, -13.51368208888610312, 71.43714994484034264 ) ) ;
#19153 = ORIENTED_EDGE ( 'NONE', *, *, #24203, .F. ) ;
#19154 = VERTEX_POINT ( 'NONE', #24438 ) ;
#19155 = DIRECTION ( 'NONE',  ( 6.489379976170840313E-31, -1.000000000000000000, 3.491481338843135327E-15 ) ) ;
#19156 = CARTESIAN_POINT ( 'NONE',  ( 32.56606138205700773, 40.39281886181299797, 84.30501292736984453 ) ) ;
#19157 = CARTESIAN_POINT ( 'NONE',  ( 39.29254315202757653, -24.80384086642191477, 72.81632618279320468 ) ) ;
#19158 = CARTESIAN_POINT ( 'NONE',  ( 42.85805032784998758, 2.782058442729017145, 6.089052160330568952 ) ) ;
#19159 = EDGE_CURVE ( 'NONE', #11585, #21184, #3060, .T. ) ;
#19160 = EDGE_LOOP ( 'NONE', ( #21981, #21898, #8720, #12485 ) ) ;
#19161 = ORIENTED_EDGE ( 'NONE', *, *, #714, .F. ) ;
#19162 = CARTESIAN_POINT ( 'NONE',  ( 28.81606138205695444, -23.19619402982950263, 47.16846523730000484 ) ) ;
#19163 = CARTESIAN_POINT ( 'NONE',  ( 31.81606138205700418, -39.60718113818700203, 82.55501292737012875 ) ) ;
#19164 = LINE ( 'NONE', #23526, #498 ) ;
#19165 = CARTESIAN_POINT ( 'NONE',  ( 39.32110845963273960, -5.470022085696077063, 83.30190618885059450 ) ) ;
#19166 = CARTESIAN_POINT ( 'NONE',  ( 32.56606138205700773, 40.39281886181299797, 82.55501292736983032 ) ) ;
#19167 = PRODUCT ( 'Upper Metal Lever Arm', 'Upper Metal Lever Arm', '', ( #3757 ) ) ;
#19168 = DIRECTION ( 'NONE',  ( -1.000000000000000000, -2.065146995210479765E-16, 1.734723475976814737E-16 ) ) ;
#19169 = ADVANCED_FACE ( 'NONE', ( #18784 ), #1123, .T. ) ;
#19170 = EDGE_LOOP ( 'NONE', ( #15133, #15496, #1393, #25466, #24597, #7501, #24802, #599 ) ) ;
#19171 = ADVANCED_FACE ( 'NONE', ( #25457 ), #1391, .F. ) ;
#19172 = LINE ( 'NONE', #5144, #4524 ) ;
#19173 = DIRECTION ( 'NONE',  ( 2.942087424212892849E-15, -0.8967398287344627850, -0.4425581086832399147 ) ) ;
#19174 = ORIENTED_EDGE ( 'NONE', *, *, #2081, .F. ) ;
#19175 = ADVANCED_FACE ( 'NONE', ( #23398 ), #7447, .F. ) ;
#19176 = ORIENTED_EDGE ( 'NONE', *, *, #5117, .T. ) ;
#19177 = CARTESIAN_POINT ( 'NONE',  ( 40.33642880535521869, -9.303840866421909439, 69.98269868914867686 ) ) ;
#19178 = EDGE_CURVE ( 'NONE', #8257, #1835, #1885, .T. ) ;
#19179 = ADVANCED_FACE ( 'NONE', ( #19289 ), #11451, .F. ) ;
#19180 = FACE_OUTER_BOUND ( 'NONE', #19023, .T. ) ;
#19181 = CARTESIAN_POINT ( 'NONE',  ( 39.75915168707250302, -12.71368208888610063, 70.26145752964251301 ) ) ;
#19182 =( LENGTH_UNIT ( ) NAMED_UNIT ( * ) SI_UNIT ( .MILLI., .METRE. ) );
#19183 = ORIENTED_EDGE ( 'NONE', *, *, #19568, .T. ) ;
#19184 = DIRECTION ( 'NONE',  ( 1.000000000000000000, 1.518641380243644581E-16, 1.055262346480601087E-16 ) ) ;
#19185 = LINE ( 'NONE', #5651, #6755 ) ;
#19186 = ADVANCED_FACE ( 'NONE', ( #1626 ), #13385, .T. ) ;
#19187 = CARTESIAN_POINT ( 'NONE',  ( 36.89935272106204422, -21.21368208888610241, 69.52238214136768590 ) ) ;
#19188 = EDGE_CURVE ( 'NONE', #12980, #19348, #23023, .T. ) ;
#19189 = EDGE_LOOP ( 'NONE', ( #2900, #8414, #15523, #20554 ) ) ;
#19190 = DIRECTION ( 'NONE',  ( -1.156482317317872711E-16, -0.4425581086832400257, 0.8967398287344628960 ) ) ;
#19191 = LINE ( 'NONE', #1523, #1203 ) ;
#19192 = LINE ( 'NONE', #1524, #512 ) ;
#19193 = CARTESIAN_POINT ( 'NONE',  ( 31.81606138205700418, 35.95440708241085304, 61.30501292736990138 ) ) ;
#19194 = DIRECTION ( 'NONE',  ( 0.000000000000000000, 1.000000000000000000, -4.625929269271481378E-15 ) ) ;
#19195 = CARTESIAN_POINT ( 'NONE',  ( 39.02742774030101458, -11.40384086642191086, 70.49320253461759478 ) ) ;
#19196 = CARTESIAN_POINT ( 'NONE',  ( 36.49096545463212493, -1.513682088886105559, 71.43714994484035685 ) ) ;
#19197 = EDGE_LOOP ( 'NONE', ( #13663, #6764, #4325, #16161 ) ) ;
#19198 = DIRECTION ( 'NONE',  ( 1.000000000000000000, 0.000000000000000000, 0.000000000000000000 ) ) ;
#19199 = DIRECTION ( 'NONE',  ( 0.000000000000000000, 0.7540134720837717852, 0.6568589528324746407 ) ) ;
#19200 = VERTEX_POINT ( 'NONE', #17363 ) ;
#19201 = ORIENTED_EDGE ( 'NONE', *, *, #25294, .T. ) ;
#19202 = CARTESIAN_POINT ( 'NONE',  ( 38.82593461698265003, -0.7038408664219141242, 73.13360434286904876 ) ) ;
#19203 = CARTESIAN_POINT ( 'NONE',  ( 39.38009889167650357, -2.213682088886108179, 72.75271321436733274 ) ) ;
#19204 = CARTESIAN_POINT ( 'NONE',  ( 40.52078840805428683, -2.613682088886105870, 70.60699637195608602 ) ) ;
#19205 = EDGE_LOOP ( 'NONE', ( #19377, #1429, #12447, #20160 ) ) ;
#19206 = DIRECTION ( 'NONE',  ( -0.000000000000000000, 0.1904761904761826663, -0.9816918156232541381 ) ) ;
#19207 = AXIS2_PLACEMENT_3D ( 'NONE', #20813, #11020, #22985 ) ;
#19208 = CARTESIAN_POINT ( 'NONE',  ( 39.24876120206129571, -4.903840866421912636, 72.12822762946750288 ) ) ;
#19209 = AXIS2_PLACEMENT_3D ( 'NONE', #5570, #3503, #3890 ) ;
#19210 = CARTESIAN_POINT ( 'NONE',  ( 40.81606138205700773, -31.05876147765399864, 75.30501292737010033 ) ) ;
#19211 = ORIENTED_EDGE ( 'NONE', *, *, #2699, .T. ) ;
#19212 = DIRECTION ( 'NONE',  ( 0.000000000000000000, 1.000000000000000000, -2.999999999999999839E-15 ) ) ;
#19213 = CARTESIAN_POINT ( 'NONE',  ( 43.81606138205700063, 35.95440708241085304, 62.30501292736990138 ) ) ;
#19214 = CARTESIAN_POINT ( 'NONE',  ( 36.29569395875881099, -12.30384086642192010, 72.77780686321128201 ) ) ;
#19215 = CARTESIAN_POINT ( 'NONE',  ( 36.72121174906109786, -21.43519715395374803, 75.33535480072937673 ) ) ;
#19216 = CARTESIAN_POINT ( 'NONE',  ( 38.26194895904383486, -17.01368208888610312, 69.64448340153877837 ) ) ;
#19217 = FACE_OUTER_BOUND ( 'NONE', #15579, .T. ) ;
#19218 = FACE_OUTER_BOUND ( 'NONE', #5878, .T. ) ;
#19219 = CARTESIAN_POINT ( 'NONE',  ( 35.14099152588522657, 1.392818861812999964, 84.30501292737000085 ) ) ;
#19220 = PRODUCT_DEFINITION ( 'UNKNOWN', '', #14986, #14181 ) ;
#19221 = CARTESIAN_POINT ( 'NONE',  ( 36.87297107704151244, -5.903840866421907307, 70.26145752964255564 ) ) ;
#19222 = VECTOR ( 'NONE', #11496, 1000.000000000000114 ) ;
#19223 = SHAPE_DEFINITION_REPRESENTATION ( #19584, #11141 ) ;
#19224 = CARTESIAN_POINT ( 'NONE',  ( 43.81606138205700063, -35.70002751211045933, 71.94742330197156832 ) ) ;
#19225 = CARTESIAN_POINT ( 'NONE',  ( 37.33957961208646736, -15.81368208888610916, 72.81632618279321889 ) ) ;
#19226 = AXIS2_PLACEMENT_3D ( 'NONE', #9138, #20586, #22392 ) ;
#19227 = CYLINDRICAL_SURFACE ( 'NONE', #6945, 0.2000000000000057288 ) ;
#19228 = CARTESIAN_POINT ( 'NONE',  ( 38.26194895904384907, -20.60384086642191548, 73.11602215082116629 ) ) ;
#19229 = CARTESIAN_POINT ( 'NONE',  ( 44.81606138205700063, 40.39281886181299797, 82.55501292736983032 ) ) ;
#19230 = CARTESIAN_POINT ( 'NONE',  ( 36.64852494920107517, -21.41368208888610525, 70.89533451361947414 ) ) ;
#19231 = EDGE_LOOP ( 'NONE', ( #8553, #16285, #11935, #24339 ) ) ;
#19232 = CARTESIAN_POINT ( 'NONE',  ( 40.55423172469004101, -1.203840866421914457, 70.70992431699450265 ) ) ;
#19233 = EDGE_LOOP ( 'NONE', ( #6921, #21719, #13873, #7047 ) ) ;
#19234 = CARTESIAN_POINT ( 'NONE',  ( 36.31606138205700063, -20.32127907754186680, 75.99695190479390305 ) ) ;
#19235 = FACE_OUTER_BOUND ( 'NONE', #8901, .T. ) ;
#19236 = CARTESIAN_POINT ( 'NONE',  ( 39.24876120206129571, -26.90384086642191264, 72.12822762946746025 ) ) ;
#19237 = VERTEX_POINT ( 'NONE', #13500 ) ;
#19238 = ORIENTED_EDGE ( 'NONE', *, *, #24901, .T. ) ;
#19239 = FACE_OUTER_BOUND ( 'NONE', #3455, .T. ) ;
#19240 = LINE ( 'NONE', #5977, #14936 ) ;
#19241 = VERTEX_POINT ( 'NONE', #7585 ) ;
#19242 = CARTESIAN_POINT ( 'NONE',  ( 43.31606138205700063, 6.355893005198818280, 6.643287643123708008 ) ) ;
#19243 = CARTESIAN_POINT ( 'NONE',  ( 37.69796330110505522, -0.5038408664219152788, 73.09843995877331224 ) ) ;
#19244 = VECTOR ( 'NONE', #18049, 1000.000000000000000 ) ;
#19245 = VECTOR ( 'NONE', #7791, 1000.000000000000000 ) ;
#19246 = VECTOR ( 'NONE', #9765, 1000.000000000000000 ) ;
#19247 = FILL_AREA_STYLE ('',( #3278 ) ) ;
#19248 = DIRECTION ( 'NONE',  ( 1.000000000000000000, 0.000000000000000000, 0.000000000000000000 ) ) ;
#19249 = ORIENTED_EDGE ( 'NONE', *, *, #4462, .T. ) ;
#19250 = EDGE_CURVE ( 'NONE', #25460, #4447, #7704, .T. ) ;
#19251 = ORIENTED_EDGE ( 'NONE', *, *, #21706, .F. ) ;
#19252 = EDGE_CURVE ( 'NONE', #13033, #24417, #5520, .T. ) ;
#19253 = DIRECTION ( 'NONE',  ( 0.000000000000000000, -0.7540134720837717852, -0.6568589528324746407 ) ) ;
#19254 = CARTESIAN_POINT ( 'NONE',  ( 44.81606138205700063, -36.05876147765410877, 70.30501292737000085 ) ) ;
#19255 = CARTESIAN_POINT ( 'NONE',  ( 39.75915168707251723, -26.90384086642191619, 72.49904802271737481 ) ) ;
#19256 = FILL_AREA_STYLE_COLOUR ( '', #5523 ) ;
#19257 = LINE ( 'NONE', #9242, #22746 ) ;
#19258 = ORIENTED_EDGE ( 'NONE', *, *, #729, .T. ) ;
#19259 = LINE ( 'NONE', #13094, #8166 ) ;
#19260 = CIRCLE ( 'NONE', #9402, 0.7500000000000006661 ) ;
#19261 = CARTESIAN_POINT ( 'NONE',  ( 30.81606138205700418, 0.3928188618129990761, 122.0250129273699997 ) ) ;
#19262 = DIRECTION ( 'NONE',  ( 1.000000000000000000, 0.000000000000000000, 0.000000000000000000 ) ) ;
#19263 = CARTESIAN_POINT ( 'NONE',  ( 37.31647492878124694, -4.303840866421912992, 72.03616607671141026 ) ) ;
#19264 = ORIENTED_EDGE ( 'NONE', *, *, #1124, .T. ) ;
#19265 = AXIS2_PLACEMENT_3D ( 'NONE', #3792, #11301, #9363 ) ;
#19266 = EDGE_CURVE ( 'NONE', #17666, #14180, #3452, .T. ) ;
#19267 = PLANE ( 'NONE',  #2089 ) ;
#19268 = ORIENTED_EDGE ( 'NONE', *, *, #21220, .F. ) ;
#19269 = EDGE_LOOP ( 'NONE', ( #21085, #14704, #6259, #8420 ) ) ;
#19270 = FACE_OUTER_BOUND ( 'NONE', #22725, .T. ) ;
#19271 = CARTESIAN_POINT ( 'NONE',  ( 37.60469502381300089, -9.213682088886100630, 70.49320253461759478 ) ) ;
#19272 = CARTESIAN_POINT ( 'NONE',  ( 38.37017380507020192, -12.01368208888610134, 72.51602215082118619 ) ) ;
#19273 = ORIENTED_EDGE ( 'NONE', *, *, #23592, .T. ) ;
#19274 = VERTEX_POINT ( 'NONE', #24933 ) ;
#19275 = CARTESIAN_POINT ( 'NONE',  ( 40.71606138205696368, -0.07962245140794542431, -2.393377716359348817 ) ) ;
#19276 = ORIENTED_EDGE ( 'NONE', *, *, #16250, .F. ) ;
#19277 = LINE ( 'NONE', #11316, #6618 ) ;
#19278 = CARTESIAN_POINT ( 'NONE',  ( 36.64852494920107517, -18.20384086642191335, 71.86517103874048473 ) ) ;
#19279 = CIRCLE ( 'NONE', #8177, 2.000000000000001776 ) ;
#19280 = DIRECTION ( 'NONE',  ( 0.000000000000000000, 0.8212051873014208914, 0.5706330172266919076 ) ) ;
#19281 = CARTESIAN_POINT ( 'NONE',  ( 37.12184278917507640, -19.51368208888610312, 71.43714994484034264 ) ) ;
#19282 = ORIENTED_EDGE ( 'NONE', *, *, #1451, .T. ) ;
#19283 = AXIS2_PLACEMENT_3D ( 'NONE', #19355, #16924, #17431 ) ;
#19284 = CARTESIAN_POINT ( 'NONE',  ( 38.57734783014581836, -5.216950748870224253, 83.30503679799366523 ) ) ;
#19285 = DIRECTION ( 'NONE',  ( 0.000000000000000000, 1.000000000000000000, 0.000000000000000000 ) ) ;
#19286 = DIRECTION ( 'NONE',  ( 0.000000000000000000, 2.775557561562888984E-15, 1.000000000000000000 ) ) ;
#19287 = VECTOR ( 'NONE', #9677, 1000.000000000000000 ) ;
#19288 = CARTESIAN_POINT ( 'NONE',  ( 39.91050633825327054, -5.989745541782124150, 83.27615889399532989 ) ) ;
#19289 = FACE_OUTER_BOUND ( 'NONE', #15896, .T. ) ;
#19290 = DIRECTION ( 'NONE',  ( 0.000000000000000000, -0.3299742535180970049, 0.9439899321577400748 ) ) ;
#19291 = ORIENTED_EDGE ( 'NONE', *, *, #3353, .F. ) ;
#19292 = CARTESIAN_POINT ( 'NONE',  ( 33.31606138205700773, 2.715274261285174351, 65.05190033008260286 ) ) ;
#19293 = ADVANCED_FACE ( 'NONE', ( #7835 ), #21350, .F. ) ;
#19294 = DIRECTION ( 'NONE',  ( 0.000000000000000000, -1.000000000000000000, 2.999999999999999839E-15 ) ) ;
#19295 = ORIENTED_EDGE ( 'NONE', *, *, #13016, .F. ) ;
#19296 = EDGE_LOOP ( 'NONE', ( #9398, #3022, #20161, #23699 ) ) ;
#19297 = CARTESIAN_POINT ( 'NONE',  ( 38.26194895904384197, -8.603840866421919031, 73.71602215082116061 ) ) ;
#19298 = VECTOR ( 'NONE', #17, 1000.000000000000114 ) ;
#19299 = LINE ( 'NONE', #5270, #6655 ) ;
#19300 = CARTESIAN_POINT ( 'NONE',  ( 38.93415946300897446, -12.11368208888610276, 73.09843995877329803 ) ) ;
#19301 = AXIS2_PLACEMENT_3D ( 'NONE', #22501, #9254, #4985 ) ;
#19302 = ORIENTED_EDGE ( 'NONE', *, *, #15691, .F. ) ;
#19303 = CARTESIAN_POINT ( 'NONE',  ( 29.81606138205694734, 5.290470704224588872, -0.3848988112044732235 ) ) ;
#19304 = DIRECTION ( 'NONE',  ( 0.000000000000000000, 2.848211695852029218E-15, 1.000000000000000000 ) ) ;
#19305 = CARTESIAN_POINT ( 'NONE',  ( 39.73277004305198545, -22.21368208888610951, 73.23812341099225875 ) ) ;
#19306 = VERTEX_POINT ( 'NONE', #19550 ) ;
#19307 = CARTESIAN_POINT ( 'NONE',  ( 43.31606138205700063, -20.88462213363798270, 44.49284693533410717 ) ) ;
#19308 = VECTOR ( 'NONE', #18652, 1000.000000000000000 ) ;
#19309 = DIRECTION ( 'NONE',  ( 6.505213034913089466E-17, -1.000000000000000000, 3.491481338843135327E-15 ) ) ;
#19310 = DIRECTION ( 'NONE',  ( -1.000000000000000000, 0.000000000000000000, 0.000000000000000000 ) ) ;
#19311 = EDGE_CURVE ( 'NONE', #19523, #16500, #22976, .T. ) ;
#19312 = ADVANCED_FACE ( 'NONE', ( #17502 ), #9652, .F. ) ;
#19313 = EDGE_CURVE ( 'NONE', #11231, #5640, #9391, .T. ) ;
#19314 = EDGE_CURVE ( 'NONE', #23124, #18988, #15296, .T. ) ;
#19315 = VECTOR ( 'NONE', #17918, 1000.000000000000000 ) ;
#19316 = CARTESIAN_POINT ( 'NONE',  ( 36.31606138205700063, -11.98739464995938953, 18.25051608701495809 ) ) ;
#19317 = CARTESIAN_POINT ( 'NONE',  ( 37.67019652925851148, -5.306778407178573964, 83.30463327861060918 ) ) ;
#19318 = AXIS2_PLACEMENT_3D ( 'NONE', #23344, #11780, #11653 ) ;
#19319 = CARTESIAN_POINT ( 'NONE',  ( 37.21915885897815457, -10.20384086642191335, 71.67976084211552745 ) ) ;
#19320 = CARTESIAN_POINT ( 'NONE',  ( 36.87297107704152666, -1.713682088886108179, 72.49904802271743165 ) ) ;
#19321 = ORIENTED_EDGE ( 'NONE', *, *, #7228, .T. ) ;
#19322 = CARTESIAN_POINT ( 'NONE',  ( 40.06556677248106269, -21.22556384466594182, 75.35168022282572053 ) ) ;
#19323 = EDGE_CURVE ( 'NONE', #23758, #3863, #15681, .T. ) ;
#19324 = DIRECTION ( 'NONE',  ( 0.000000000000000000, 0.5706330172266919076, -0.8212051873014208914 ) ) ;
#19325 = ORIENTED_EDGE ( 'NONE', *, *, #22162, .T. ) ;
#19326 = EDGE_CURVE ( 'NONE', #16812, #21490, #13761, .T. ) ;
#19327 = ORIENTED_EDGE ( 'NONE', *, *, #18283, .T. ) ;
#19328 = CIRCLE ( 'NONE', #15225, 0.5000000000000011102 ) ;
#19329 = CARTESIAN_POINT ( 'NONE',  ( 38.93415946300896024, -1.503840866421908729, 69.66206559358663242 ) ) ;
#19330 = CARTESIAN_POINT ( 'NONE',  ( 38.73920764526925353, -28.11368208888610454, 72.49843995877328950 ) ) ;
#19331 = CARTESIAN_POINT ( 'NONE',  ( 36.29569395875879678, -1.313682088886099830, 69.98269868914869107 ) ) ;
#19332 = ORIENTED_EDGE ( 'NONE', *, *, #3907, .T. ) ;
#19333 = DIRECTION ( 'NONE',  ( 1.000000000000000000, 0.000000000000000000, 0.000000000000000000 ) ) ;
#19334 = CARTESIAN_POINT ( 'NONE',  ( 37.60469502381300799, -2.403840866421910416, 72.26730301774236409 ) ) ;
#19335 = APPLICATION_CONTEXT ( 'automotive_design' ) ;
#19336 = LINE ( 'NONE', #9693, #19222 ) ;
#19337 = ORIENTED_EDGE ( 'NONE', *, *, #8169, .F. ) ;
#19338 = CARTESIAN_POINT ( 'NONE',  ( 32.81606138205700773, -34.55876147765403061, 66.30501292737011454 ) ) ;
#19339 = DIRECTION ( 'NONE',  ( 0.000000000000000000, 0.8212051873014208914, 0.5706330172266919076 ) ) ;
#19340 = CARTESIAN_POINT ( 'NONE',  ( 38.26194895904384197, -8.603840866421919031, 73.71602215082116061 ) ) ;
#19341 = DIRECTION ( 'NONE',  ( 0.000000000000000000, 1.000000000000000000, 0.000000000000000000 ) ) ;
#19342 = CARTESIAN_POINT ( 'NONE',  ( 39.38009889167650357, -12.21368208888610596, 72.75271321436731853 ) ) ;
#19343 = CARTESIAN_POINT ( 'NONE',  ( 40.31606138205701484, -21.83924545618508617, 28.60179643084732604 ) ) ;
#19344 = CIRCLE ( 'NONE', #22639, 4.000000000000003553 ) ;
#19345 = CYLINDRICAL_SURFACE ( 'NONE', #2334, 1.500000000000001332 ) ;
#19346 = VECTOR ( 'NONE', #24157, 1000.000000000000000 ) ;
#19347 = EDGE_CURVE ( 'NONE', #21396, #20637, #22111, .T. ) ;
#19348 = VERTEX_POINT ( 'NONE', #4095 ) ;
#19349 = EDGE_CURVE ( 'NONE', #3431, #13994, #14140, .T. ) ;
#19350 = CARTESIAN_POINT ( 'NONE',  ( 45.81606138205700063, 39.39281886181299797, 81.75501292736983316 ) ) ;
#19351 = CARTESIAN_POINT ( 'NONE',  ( 38.26194895904384907, -10.60384086642191726, 73.11602215082118050 ) ) ;
#19352 = SHAPE_DEFINITION_REPRESENTATION ( #13630, #4169 ) ;
#19353 = FACE_OUTER_BOUND ( 'NONE', #3728, .T. ) ;
#19354 = CARTESIAN_POINT ( 'NONE',  ( 36.87297107704152666, -17.71368208888610951, 72.49904802271740323 ) ) ;
#19355 = CARTESIAN_POINT ( 'NONE',  ( 39.81746892067405952, 41.67000142393845152, 79.87823623207322044 ) ) ;
#19356 = EDGE_CURVE ( 'NONE', #3300, #21877, #14001, .T. ) ;
#19357 = CARTESIAN_POINT ( 'NONE',  ( 38.26194895904384907, -18.60384086642191548, 73.11602215082116629 ) ) ;
#19358 = CARTESIAN_POINT ( 'NONE',  ( 37.09309150775561648, -5.596673503582127118, 82.79754871965852203 ) ) ;
#19359 = CARTESIAN_POINT ( 'NONE',  ( 39.29254315202756231, -20.81368208888610027, 69.94417936956672577 ) ) ;
#19360 = ORIENTED_EDGE ( 'NONE', *, *, #16077, .T. ) ;
#19361 = CARTESIAN_POINT ( 'NONE',  ( 37.61123632939165873, -21.91368208888611235, 73.73360434286898624 ) ) ;
#19362 = VERTEX_POINT ( 'NONE', #14013 ) ;
#19363 = CARTESIAN_POINT ( 'NONE',  ( 30.81606138205700418, -38.55876147765410167, 72.21586839016130455 ) ) ;
#19364 = CARTESIAN_POINT ( 'NONE',  ( 31.81606138205700418, 18.19123852234599426, 73.05501292736995822 ) ) ;
#19365 = AXIS2_PLACEMENT_3D ( 'NONE', #24531, #6789, #2772 ) ;
#19366 = CARTESIAN_POINT ( 'NONE',  ( 39.41296390513587511, -25.20384086642191335, 71.08074471024438878 ) ) ;
#19367 = EDGE_LOOP ( 'NONE', ( #5180, #6917, #8336, #22682, #15583, #5970, #2711, #22435, #22577, #14291, #19268, #20806 ) ) ;
#19368 = ADVANCED_FACE ( 'NONE', ( #10273 ), #18009, .F. ) ;
#19369 = VERTEX_POINT ( 'NONE', #7968 ) ;
#19370 = CARTESIAN_POINT ( 'NONE',  ( 39.66066260159757917, -29.10876147765399580, 70.75778293607493197 ) ) ;
#19371 = LINE ( 'NONE', #17702, #1361 ) ;
#19372 = EDGE_LOOP ( 'NONE', ( #11341, #9627, #4906, #7842 ) ) ;
#19373 = DIRECTION ( 'NONE',  ( 1.000000000000000000, 2.973811673103095397E-15, 0.000000000000000000 ) ) ;
#19374 = CARTESIAN_POINT ( 'NONE',  ( 38.26194895904384197, -28.60384086642191548, 73.71602215082113219 ) ) ;
#19375 = PRODUCT ( 'Staple Pusher', 'Staple Pusher', '', ( #7764 ) ) ;
#19376 = CARTESIAN_POINT ( 'NONE',  ( 40.56606138205700773, 5.594015759443068170, 2.006005027196319901 ) ) ;
#19377 = ORIENTED_EDGE ( 'NONE', *, *, #2925, .F. ) ;
#19378 = ORIENTED_EDGE ( 'NONE', *, *, #3773, .F. ) ;
#19379 = CARTESIAN_POINT ( 'NONE',  ( 37.31606138205700063, 43.19123852234599781, 74.30501292736987295 ) ) ;
#19380 = DIRECTION ( 'NONE',  ( -0.000000000000000000, -0.1330350631819583740, 0.9911113317706403691 ) ) ;
#19381 = DIRECTION ( 'NONE',  ( -0.000000000000000000, -3.469446951953613400E-15, -1.000000000000000000 ) ) ;
#19382 = FACE_OUTER_BOUND ( 'NONE', #4732, .T. ) ;
#19383 = AXIS2_PLACEMENT_3D ( 'NONE', #21337, #1493, #13115 ) ;
#19384 = EDGE_LOOP ( 'NONE', ( #22668, #20615, #13076, #16194 ) ) ;
#19385 = CARTESIAN_POINT ( 'NONE',  ( 40.31606138205701484, -19.58709462196289763, 24.03834292329984379 ) ) ;
#19386 = PLANE ( 'NONE',  #8640 ) ;
#19387 = CARTESIAN_POINT ( 'NONE',  ( 33.31606138205700773, 6.705285648480822758, 7.416521610403067122 ) ) ;
#19388 = CARTESIAN_POINT ( 'NONE',  ( 39.37952058850012804, -9.003840866421910505, 71.78268878715392987 ) ) ;
#19389 = EDGE_LOOP ( 'NONE', ( #3799, #12246, #9655, #3868 ) ) ;
#19390 = CARTESIAN_POINT ( 'NONE',  ( 45.81606138205697221, -4.589472609077215104, -6.350807634294792337 ) ) ;
#19391 = ORIENTED_EDGE ( 'NONE', *, *, #18197, .T. ) ;
#19392 = ORIENTED_EDGE ( 'NONE', *, *, #4401, .T. ) ;
#19394 = ADVANCED_FACE ( 'NONE', ( #2141 ), #2397, .F. ) ;
#19393 = CARTESIAN_POINT ( 'NONE',  ( 31.81606138205700418, 38.19123852234598360, 71.05501292736988717 ) ) ;
#19395 = CARTESIAN_POINT ( 'NONE',  ( 37.12184278917507640, -11.51368208888610134, 71.43714994484034264 ) ) ;
#19396 = EDGE_CURVE ( 'NONE', #12037, #5642, #210, .T. ) ;
#19397 = CARTESIAN_POINT ( 'NONE',  ( 39.31564783533280405, -8.313682088886102051, 72.03616607671141026 ) ) ;
#19398 = ORIENTED_EDGE ( 'NONE', *, *, #15153, .T. ) ;
#19399 = EDGE_CURVE ( 'NONE', #58, #7231, #8344, .T. ) ;
#19400 = ORIENTED_EDGE ( 'NONE', *, *, #13016, .T. ) ;
#19401 = CARTESIAN_POINT ( 'NONE',  ( 41.14099152588523367, 1.392818861812999964, 93.30501292736998664 ) ) ;
#19402 = FACE_OUTER_BOUND ( 'NONE', #18900, .T. ) ;
#19403 = VERTEX_POINT ( 'NONE', #16186 ) ;
#19404 = CARTESIAN_POINT ( 'NONE',  ( 38.31606138205700063, 42.51966564709218233, 70.30501292737018559 ) ) ;
#19405 = CARTESIAN_POINT ( 'NONE',  ( 36.49096545463212493, -20.10384086642191193, 71.32335560751961623 ) ) ;
#19406 = DIRECTION ( 'NONE',  ( 0.000000000000000000, 6.469446951953614816E-15, 1.000000000000000000 ) ) ;
#19407 = CARTESIAN_POINT ( 'NONE',  ( 37.60469502381300089, -17.21368208888610241, 70.49320253461759478 ) ) ;
#19408 = ORIENTED_EDGE ( 'NONE', *, *, #22431, .T. ) ;
#19409 = CARTESIAN_POINT ( 'NONE',  ( 43.39391466435857581, 3.105264735554318811, 6.136852473770198380 ) ) ;
#19410 = DIRECTION ( 'NONE',  ( 0.000000000000000000, -1.000000000000000000, 3.304235192336775512E-15 ) ) ;
#19411 = CARTESIAN_POINT ( 'NONE',  ( 33.31606138205700773, 8.791238522312193382, 67.36094597237627113 ) ) ;
#19412 = CARTESIAN_POINT ( 'NONE',  ( 39.64148445914975127, -5.700736305954877459, 83.29367725972169012 ) ) ;
#19413 = CARTESIAN_POINT ( 'NONE',  ( 35.31606138205700773, 3.195231713396695650, 64.80689721350518084 ) ) ;
#19414 = VECTOR ( 'NONE', #23677, 1000.000000000000000 ) ;
#19415 = CARTESIAN_POINT ( 'NONE',  ( 35.14099152588522657, 40.39281886181299797, 84.30501292736984453 ) ) ;
#19416 = ORIENTED_EDGE ( 'NONE', *, *, #14064, .F. ) ;
#19417 = DIRECTION ( 'NONE',  ( 0.000000000000000000, -2.999999999999999839E-15, -1.000000000000000000 ) ) ;
#19418 = ORIENTED_EDGE ( 'NONE', *, *, #24621, .F. ) ;
#19419 = ORIENTED_EDGE ( 'NONE', *, *, #391, .F. ) ;
#19420 = CARTESIAN_POINT ( 'NONE',  ( 36.36258059203030513, -7.903840866421910860, 69.89063713639259845 ) ) ;
#19421 = ORIENTED_EDGE ( 'NONE', *, *, #11969, .F. ) ;
#19422 = LINE ( 'NONE', #15822, #21065 ) ;
#19423 = CARTESIAN_POINT ( 'NONE',  ( 36.68196826583682935, -13.61368208888610454, 71.96809898377888715 ) ) ;
#19424 = SURFACE_STYLE_FILL_AREA ( #3465 ) ;
#19425 = ORIENTED_EDGE ( 'NONE', *, *, #2006, .F. ) ;
#19426 = CARTESIAN_POINT ( 'NONE',  ( 33.63430007298546087, 2.841684771932709186, 6.101742786271089791 ) ) ;
#19427 = DIRECTION ( 'NONE',  ( 0.000000000000000000, -1.000000000000000000, 2.999999999999999839E-15 ) ) ;
#19428 = CARTESIAN_POINT ( 'NONE',  ( 40.55423172469004811, -22.41368208888610525, 72.05058123536544201 ) ) ;
#19429 = ORIENTED_EDGE ( 'NONE', *, *, #16732, .F. ) ;
#19430 = VECTOR ( 'NONE', #25454, 1000.000000000000227 ) ;
#19431 = CARTESIAN_POINT ( 'NONE',  ( 31.81606138205700418, 40.39281886181299797, 66.30501292737000085 ) ) ;
#19432 = DIRECTION ( 'NONE',  ( -1.000000000000000000, 0.000000000000000000, 0.000000000000000000 ) ) ;
#19433 = DIRECTION ( 'NONE',  ( 0.000000000000000000, -0.4425581086832400257, 0.8967398287344627850 ) ) ;
#19434 = ADVANCED_FACE ( 'NONE', ( #19675 ), #2270, .F. ) ;
#19435 = VECTOR ( 'NONE', #20301, 1000.000000000000114 ) ;
#19436 = LINE ( 'NONE', #17649, #20322 ) ;
#19437 = CARTESIAN_POINT ( 'NONE',  ( 34.56606138205700773, 43.19123852234599781, 75.30501292736987295 ) ) ;
#19438 = AXIS2_PLACEMENT_3D ( 'NONE', #20844, #18526, #9001 ) ;
#19439 = CIRCLE ( 'NONE', #8359, 1.750000000000001554 ) ;
#19440 = CARTESIAN_POINT ( 'NONE',  ( 36.57819145821473228, -6.205787318996375035, 83.25770116091617012 ) ) ;
#19441 = CARTESIAN_POINT ( 'NONE',  ( 38.26194895904384197, -14.60384086642191193, 72.51602215082118619 ) ) ;
#19442 = CARTESIAN_POINT ( 'NONE',  ( 38.37017380507020192, 1.986317911113890444, 73.11602215082119471 ) ) ;
#19443 = ORIENTED_EDGE ( 'NONE', *, *, #479, .F. ) ;
#19444 = CARTESIAN_POINT ( 'NONE',  ( 33.31606138205700773, 3.195231713396695650, 64.80689721350518084 ) ) ;
#19445 = VECTOR ( 'NONE', #18341, 1000.000000000000000 ) ;
#19446 = CARTESIAN_POINT ( 'NONE',  ( 44.81606138205700063, -38.55876147765401640, 70.30501292737012875 ) ) ;
#19447 = ORIENTED_EDGE ( 'NONE', *, *, #12413, .F. ) ;
#19448 = ORIENTED_EDGE ( 'NONE', *, *, #22490, .F. ) ;
#19449 = VECTOR ( 'NONE', #5605, 1000.000000000000000 ) ;
#19450 = CARTESIAN_POINT ( 'NONE',  ( 36.49096545463212493, -0.1038408664219107880, 71.32335560751963044 ) ) ;
#19451 = EDGE_CURVE ( 'NONE', #17509, #3532, #10146, .T. ) ;
#19452 = EDGE_CURVE ( 'NONE', #16039, #17020, #15811, .T. ) ;
#19453 = AXIS2_PLACEMENT_3D ( 'NONE', #13209, #3142, #12705 ) ;
#19454 = CARTESIAN_POINT ( 'NONE',  ( 39.98359781491296161, 1.586317911113896528, 71.86517103874049894 ) ) ;
#19455 = CARTESIAN_POINT ( 'NONE',  ( 37.61123632939165873, 0.08631791111389161553, 73.73360434286902887 ) ) ;
#19456 = ORIENTED_EDGE ( 'NONE', *, *, #22431, .F. ) ;
#19457 = CARTESIAN_POINT ( 'NONE',  ( 33.31606138205700773, -19.34822312381090370, 24.15308711316412627 ) ) ;
#19458 = CARTESIAN_POINT ( 'NONE',  ( 37.25260217561390874, -4.003840866421911393, 70.97781676520604321 ) ) ;
#19459 = ADVANCED_FACE ( 'NONE', ( #6154, #16060 ), #2519, .F. ) ;
#19460 = FACE_OUTER_BOUND ( 'NONE', #742, .T. ) ;
#19461 = ORIENTED_EDGE ( 'NONE', *, *, #21210, .F. ) ;
#19462 = AXIS2_PLACEMENT_3D ( 'NONE', #9384, #23392, #1747 ) ;
#19463 = FACE_OUTER_BOUND ( 'NONE', #25409, .T. ) ;
#19464 = LINE ( 'NONE', #21273, #21545 ) ;
#19465 = CARTESIAN_POINT ( 'NONE',  ( 39.12911128074872380, -11.50384086642191050, 69.06206559358666652 ) ) ;
#19466 = DIRECTION ( 'NONE',  ( -1.000000000000000000, 0.000000000000000000, 0.000000000000000000 ) ) ;
#19467 = CARTESIAN_POINT ( 'NONE',  ( 38.26194895904383486, -13.01368208888610134, 69.64448340153877837 ) ) ;
#19468 = DIRECTION ( 'NONE',  ( 0.000000000000000000, -0.7540134720837682325, -0.6568589528324786375 ) ) ;
#19469 = ADVANCED_FACE ( 'NONE', ( #16301 ), #1984, .T. ) ;
#19470 = CARTESIAN_POINT ( 'NONE',  ( 45.81606138205700063, -34.55876147765410167, 70.30501292737000085 ) ) ;
#19471 = AXIS2_PLACEMENT_3D ( 'NONE', #22456, #22840, #18848 ) ;
#19472 = DIRECTION ( 'NONE',  ( 0.000000000000000000, 1.000000000000000000, 0.000000000000000000 ) ) ;
#19473 = AXIS2_PLACEMENT_3D ( 'NONE', #3615, #15471, #13303 ) ;
#19474 = CARTESIAN_POINT ( 'NONE',  ( 40.14115730948191185, 0.8961591335780899614, 71.43714994484035685 ) ) ;
#19475 = ITEM_DEFINED_TRANSFORMATION ( 'NONE', 'NONE', #25260,  #2000 ) ;
#19476 = CARTESIAN_POINT ( 'NONE',  ( 40.81606138205700773, -29.78523130861184143, 52.92072663988442116 ) ) ;
#19477 = CARTESIAN_POINT ( 'NONE',  ( 36.80608444377001121, -21.31368208888610027, 70.35351908239857721 ) ) ;
#19478 = DIRECTION ( 'NONE',  ( -1.000000000000000000, -2.440719103442460517E-15, -1.328886038262201063E-15 ) ) ;
#19479 = VECTOR ( 'NONE', #103, 1000.000000000000000 ) ;
#19480 = CARTESIAN_POINT ( 'NONE',  ( 40.14115730948191185, -17.10384086642191193, 71.43714994484030001 ) ) ;
#19481 = ADVANCED_FACE ( 'NONE', ( #3963 ), #20092, .F. ) ;
#19482 = DIRECTION ( 'NONE',  ( -1.000000000000000000, 0.000000000000000000, 0.000000000000000000 ) ) ;
#19483 = MECHANICAL_DESIGN_GEOMETRIC_PRESENTATION_REPRESENTATION (  '', ( #5123 ), #552 ) ;
#19484 = EDGE_CURVE ( 'NONE', #559, #786, #6525, .T. ) ;
#19485 = CARTESIAN_POINT ( 'NONE',  ( 36.87297107704152666, -19.71368208888610951, 72.49904802271740323 ) ) ;
#19486 = ORIENTED_EDGE ( 'NONE', *, *, #20058, .T. ) ;
#19487 = CARTESIAN_POINT ( 'NONE',  ( 40.52078840805428683, -20.61368208888610454, 70.60699637195608602 ) ) ;
#19488 = ORIENTED_EDGE ( 'NONE', *, *, #25429, .F. ) ;
#19489 = DIRECTION ( 'NONE',  ( 0.000000000000000000, 0.000000000000000000, 1.000000000000000000 ) ) ;
#19490 = EDGE_CURVE ( 'NONE', #23735, #6436, #11463, .T. ) ;
#19491 = AXIS2_PLACEMENT_3D ( 'NONE', #14565, #2954, #18320 ) ;
#19492 = CARTESIAN_POINT ( 'NONE',  ( 40.64099152588523367, 1.142818861812999742, 93.30501292736998664 ) ) ;
#19493 = CARTESIAN_POINT ( 'NONE',  ( 37.38336156205273397, -23.90384086642191619, 70.63227792289245599 ) ) ;
#19494 = EDGE_CURVE ( 'NONE', #7168, #13296, #6931, .T. ) ;
#19495 = EDGE_CURVE ( 'NONE', #11605, #9789, #5288, .T. ) ;
#19496 = VECTOR ( 'NONE', #22547, 1000.000000000000000 ) ;
#19497 = ORIENTED_EDGE ( 'NONE', *, *, #4182, .T. ) ;
#19498 = VERTEX_POINT ( 'NONE', #16432 ) ;
#19499 = CARTESIAN_POINT ( 'NONE',  ( 39.65020039316494405, -29.05171021479125315, 70.79984939021886703 ) ) ;
#19500 = CARTESIAN_POINT ( 'NONE',  ( 43.31606138205700063, 7.166937456968672571, 6.752152658007350539 ) ) ;
#19501 = ORIENTED_EDGE ( 'NONE', *, *, #17581, .F. ) ;
#19502 =( LENGTH_UNIT ( ) NAMED_UNIT ( * ) SI_UNIT ( .MILLI., .METRE. ) );
#19503 = CARTESIAN_POINT ( 'NONE',  ( 36.68196826583682935, -0.003840866421911393047, 70.79240656858108593 ) ) ;
#19504 = DIRECTION ( 'NONE',  ( 0.000000000000000000, -0.5706330172266907974, 0.8212051873014217795 ) ) ;
#19505 = CARTESIAN_POINT ( 'NONE',  ( 36.36258059203031934, -3.713682088886109955, 72.86986841596736042 ) ) ;
#19506 = EDGE_CURVE ( 'NONE', #2232, #8221, #24283, .T. ) ;
#19507 = DIRECTION ( 'NONE',  ( 1.000000000000000000, 2.999999999999999839E-15, 0.000000000000000000 ) ) ;
#19508 = ADVANCED_FACE ( 'NONE', ( #18757 ), #22492, .T. ) ;
#19509 = ORIENTED_EDGE ( 'NONE', *, *, #9562, .F. ) ;
#19510 = VERTEX_POINT ( 'NONE', #24660 ) ;
#19511 = CARTESIAN_POINT ( 'NONE',  ( 43.31606138205700063, -29.06829118875199924, 75.30501292737000085 ) ) ;
#19512 = DIRECTION ( 'NONE',  ( 0.000000000000000000, -1.000000000000000000, 2.999999999999999839E-15 ) ) ;
#19513 = CARTESIAN_POINT ( 'NONE',  ( 38.26194895904384907, -20.60384086642191548, 73.11602215082116629 ) ) ;
#19514 = VECTOR ( 'NONE', #787, 1000.000000000000000 ) ;
#19515 =( LENGTH_UNIT ( ) NAMED_UNIT ( * ) SI_UNIT ( .MILLI., .METRE. ) );
#19516 = CARTESIAN_POINT ( 'NONE',  ( 43.31606138205700063, 7.282926244446933595, 65.60596383066929604 ) ) ;
#19517 = ORIENTED_EDGE ( 'NONE', *, *, #6928, .T. ) ;
#19518 = DIRECTION ( 'NONE',  ( 0.000000000000000000, 0.000000000000000000, -1.000000000000000000 ) ) ;
#19519 = AXIS2_PLACEMENT_3D ( 'NONE', #9977, #9477, #4175 ) ;
#19520 = CARTESIAN_POINT ( 'NONE',  ( 29.71606138205694947, 1.152853241805954498, -2.169147274601580744 ) ) ;
#19521 = DIRECTION ( 'NONE',  ( 1.734723475976805517E-15, -0.4425581086832399702, 0.8967398287344627850 ) ) ;
#19522 = CARTESIAN_POINT ( 'NONE',  ( 39.41296390513587511, -5.203840866421910683, 71.08074471024443142 ) ) ;
#19523 = VERTEX_POINT ( 'NONE', #10531 ) ;
#19524 = DIRECTION ( 'NONE',  ( -2.163881430871171154E-15, 0.7573960774932753104, -0.6529557272876933549 ) ) ;
#19525 = EDGE_LOOP ( 'NONE', ( #9303, #21620, #8451, #16193 ) ) ;
#19526 = ORIENTED_EDGE ( 'NONE', *, *, #17911, .T. ) ;
#19527 = DIRECTION ( 'NONE',  ( 0.000000000000000000, 0.7540134720837717852, 0.6568589528324746407 ) ) ;
#19528 = CARTESIAN_POINT ( 'NONE',  ( 38.93987200065208754, -14.81368208888610205, 70.42958956619168021 ) ) ;
#19529 = AXIS2_PLACEMENT_3D ( 'NONE', #22332, #10994, #3124 ) ;
#19530 = CARTESIAN_POINT ( 'NONE',  ( 39.37952058850012804, -8.613682088886100985, 70.97781676520601479 ) ) ;
#19531 = ORIENTED_EDGE ( 'NONE', *, *, #1226, .F. ) ;
#19532 = EDGE_LOOP ( 'NONE', ( #16530, #14367, #959, #13442, #9992, #17203, #21205, #13006, #23250, #24746, #755, #19258, #8313, #1335, #21621, #24 ) ) ;
#19533 = CYLINDRICAL_SURFACE ( 'NONE', #8693, 1.000000000000000888 ) ;
#19534 = DIRECTION ( 'NONE',  ( 1.000000000000000000, 0.000000000000000000, 0.000000000000000000 ) ) ;
#19535 = ORIENTED_EDGE ( 'NONE', *, *, #891, .F. ) ;
#19536 = DIRECTION ( 'NONE',  ( 0.000000000000000000, -0.8967398287344635621, -0.4425581086832386379 ) ) ;
#19537 = CARTESIAN_POINT ( 'NONE',  ( 36.64852494920107517, -20.20384086642191335, 71.86517103874048473 ) ) ;
#19538 = VECTOR ( 'NONE', #18336, 1000.000000000000000 ) ;
#19539 = CARTESIAN_POINT ( 'NONE',  ( 42.82341778883947825, 3.225255403573667135, 6.370938332379879832 ) ) ;
#19540 = CARTESIAN_POINT ( 'NONE',  ( 38.93987200065208754, -16.81368208888610383, 70.42958956619168021 ) ) ;
#19541 = ORIENTED_EDGE ( 'NONE', *, *, #18529, .F. ) ;
#19542 = ORIENTED_EDGE ( 'NONE', *, *, #10888, .T. ) ;
#19543 = DIRECTION ( 'NONE',  ( 2.792262043613788535E-15, -0.8967398287344626739, -0.4425581086832399147 ) ) ;
#19544 = CARTESIAN_POINT ( 'NONE',  ( 39.95015449827720744, -16.61368208888610454, 70.79240656858105751 ) ) ;
#19545 = DIRECTION ( 'NONE',  ( 0.000000000000000000, -0.8212051873014203363, -0.5706330172266926848 ) ) ;
#19546 = ADVANCED_FACE ( 'NONE', ( #10657 ), #708, .T. ) ;
#19547 = CARTESIAN_POINT ( 'NONE',  ( 40.56606138205700773, 5.719301844480432884, 2.701924129460374413 ) ) ;
#19548 = ADVANCED_FACE ( 'NONE', ( #18627 ), #12973, .T. ) ;
#19549 = CARTESIAN_POINT ( 'NONE',  ( 31.81606138205700418, -36.55876147765401640, 71.30501292737011454 ) ) ;
#19550 = CARTESIAN_POINT ( 'NONE',  ( 33.31606138205700773, -5.204193249396280585, 82.80501292736992980 ) ) ;
#19551 = AXIS2_PLACEMENT_3D ( 'NONE', #19718, #17412, #3614 ) ;
#19552 = DIRECTION ( 'NONE',  ( 1.000000000000000000, 1.156482317317870344E-15, 0.000000000000000000 ) ) ;
#19553 = VERTEX_POINT ( 'NONE', #8854 ) ;
#19554 = CARTESIAN_POINT ( 'NONE',  ( 44.81606138205700063, 34.87886987267150118, 84.30501292736984453 ) ) ;
#19555 = VERTEX_POINT ( 'NONE', #24527 ) ;
#19556 = EDGE_LOOP ( 'NONE', ( #19785, #12070, #4785, #3166 ) ) ;
#19557 = CARTESIAN_POINT ( 'NONE',  ( 36.07789103942399578, -10.20384086642191690, 72.05058123536544201 ) ) ;
#19558 = ORIENTED_EDGE ( 'NONE', *, *, #12228, .F. ) ;
#19559 = LINE ( 'NONE', #21748, #11616 ) ;
#19560 = CARTESIAN_POINT ( 'NONE',  ( 37.69796330110504101, -17.11368208888610098, 69.66206559358661821 ) ) ;
#19561 = VERTEX_POINT ( 'NONE', #16953 ) ;
#19562 = DIRECTION ( 'NONE',  ( -1.000000000000000000, 5.204170427930413997E-31, 1.734723475976804876E-16 ) ) ;
#19563 = DIRECTION ( 'NONE',  ( -2.122643018205887308E-17, 1.000000000000000000, -3.120611096041553009E-15 ) ) ;
#19564 = CARTESIAN_POINT ( 'NONE',  ( 40.77203464402485622, -18.51368208888610312, 71.32335560751960202 ) ) ;
#19565 = VERTEX_POINT ( 'NONE', #6907 ) ;
#19566 = LINE ( 'NONE', #15448, #20138 ) ;
#19567 = CARTESIAN_POINT ( 'NONE',  ( 40.81606138205700773, -31.05876147765399864, 75.30501292737010033 ) ) ;
#19568 = EDGE_CURVE ( 'NONE', #6874, #5497, #11029, .T. ) ;
#19569 = CARTESIAN_POINT ( 'NONE',  ( 44.81606138205700063, -3.831401139557048197, 80.75501292737000369 ) ) ;
#19570 =( NAMED_UNIT ( * ) PLANE_ANGLE_UNIT ( ) SI_UNIT ( $, .RADIAN. ) );
#19571 = EDGE_CURVE ( 'NONE', #11291, #12560, #22619, .T. ) ;
#19572 = DIRECTION ( 'NONE',  ( -1.000000000000000000, -2.999999999999999839E-15, 0.000000000000000000 ) ) ;
#19573 = DIRECTION ( 'NONE',  ( 0.000000000000000000, 1.000000000000000000, -2.775557561562891351E-15 ) ) ;
#19574 = CARTESIAN_POINT ( 'NONE',  ( 37.31647492878124694, -14.30384086642191122, 72.03616607671141026 ) ) ;
#19575 = CARTESIAN_POINT ( 'NONE',  ( 37.25260217561390874, -27.61368208888610454, 71.78268878715390144 ) ) ;
#19576 = ORIENTED_EDGE ( 'NONE', *, *, #18801, .F. ) ;
#19577 = DIRECTION ( 'NONE',  ( 1.000000000000000000, -5.204170427930415223E-30, -1.734723475976805122E-15 ) ) ;
#19578 = FACE_OUTER_BOUND ( 'NONE', #19205, .T. ) ;
#19579 = ORIENTED_EDGE ( 'NONE', *, *, #10698, .T. ) ;
#19580 = ORIENTED_EDGE ( 'NONE', *, *, #18675, .F. ) ;
#19581 = CARTESIAN_POINT ( 'NONE',  ( 36.98690846071097127, -27.80384086642191477, 69.45876917294174291 ) ) ;
#19582 = EDGE_CURVE ( 'NONE', #25398, #7168, #7033, .T. ) ;
#19583 = CARTESIAN_POINT ( 'NONE',  ( 37.89291511884476904, -25.11368208888610454, 70.26206559358661252 ) ) ;
#19584 = PRODUCT_DEFINITION_SHAPE ( 'NONE', 'NONE',  #19220 ) ;
#19585 = CARTESIAN_POINT ( 'NONE',  ( 40.52078840805428683, -4.613682088886104538, 70.60699637195608602 ) ) ;
#19586 = ORIENTED_EDGE ( 'NONE', *, *, #15151, .T. ) ;
#19587 = LINE ( 'NONE', #5556, #11962 ) ;
#19588 = CARTESIAN_POINT ( 'NONE',  ( 39.37952058850012804, -7.003840866421911393, 71.78268878715392987 ) ) ;
#19589 = CARTESIAN_POINT ( 'NONE',  ( 42.81606138205700063, 16.19123852234699967, 69.30501292736995822 ) ) ;
#19590 = ORIENTED_EDGE ( 'NONE', *, *, #7843, .F. ) ;
#19591 = CARTESIAN_POINT ( 'NONE',  ( 30.81606138205697931, -5.918777154956195830, -5.916875169744970187 ) ) ;
#19592 = CARTESIAN_POINT ( 'NONE',  ( 46.81606138205697221, -4.349482454670835274, -5.142398479549302515 ) ) ;
#19593 = CARTESIAN_POINT ( 'NONE',  ( 40.55423172469004101, -13.20384086642191690, 70.70992431699450265 ) ) ;
#19594 = CARTESIAN_POINT ( 'NONE',  ( 33.31606138205700773, -21.50052602411404834, 44.06487217241408416 ) ) ;
#19595 = LINE ( 'NONE', #21405, #1693 ) ;
#19596 = CARTESIAN_POINT ( 'NONE',  ( 39.29254315202756231, -12.81368208888610383, 69.94417936956672577 ) ) ;
#19597 = DIRECTION ( 'NONE',  ( -1.000000000000000000, -2.967680473743455856E-15, -2.960622826238914985E-16 ) ) ;
#19598 = LINE ( 'NONE', #1939, #8517 ) ;
#19599 = DIRECTION ( 'NONE',  ( 0.000000000000000000, -1.000000000000000000, 0.000000000000000000 ) ) ;
#19600 = CARTESIAN_POINT ( 'NONE',  ( 40.14115730948191185, -1.103840866421911482, 71.43714994484034264 ) ) ;
#19601 = CONTEXT_DEPENDENT_SHAPE_REPRESENTATION ( #8330, #2460 ) ;
#19602 = CARTESIAN_POINT ( 'NONE',  ( 33.31606138205700773, -13.58280000135114030, 20.54174511886706256 ) ) ;
#19603 = CARTESIAN_POINT ( 'NONE',  ( 36.87297107704152666, -19.71368208888610951, 72.49904802271740323 ) ) ;
#19604 = CARTESIAN_POINT ( 'NONE',  ( 32.81606138205700773, -36.55876147765401640, 71.30501292737011454 ) ) ;
#19605 = CARTESIAN_POINT ( 'NONE',  ( 38.82593461698265003, -18.70384086642191690, 73.13360434286903455 ) ) ;
#19606 = DIRECTION ( 'NONE',  ( 1.000000000000000000, 0.000000000000000000, 0.000000000000000000 ) ) ;
#19607 = VECTOR ( 'NONE', #8816, 1000.000000000000000 ) ;
#19608 = CARTESIAN_POINT ( 'NONE',  ( 36.80608444377001121, -13.31368208888609672, 70.35351908239857721 ) ) ;
#19609 = ORIENTED_EDGE ( 'NONE', *, *, #9425, .F. ) ;
#19610 = CARTESIAN_POINT ( 'NONE',  ( 40.26954217208371034, -24.71368208888610241, 69.89063713639254161 ) ) ;
#19611 = VERTEX_POINT ( 'NONE', #12472 ) ;
#19612 = LINE ( 'NONE', #21296, #20560 ) ;
#19613 = CARTESIAN_POINT ( 'NONE',  ( 43.31606138205700773, -18.80550481115970740, 25.27912300651437150 ) ) ;
#19614 = CARTESIAN_POINT ( 'NONE',  ( 38.00113996487112189, -25.70384086642191690, 70.22690120949089021 ) ) ;
#19615 = ORIENTED_EDGE ( 'NONE', *, *, #20927, .F. ) ;
#19616 = ORIENTED_EDGE ( 'NONE', *, *, #14158, .F. ) ;
#19617 = DIRECTION ( 'NONE',  ( -1.000000000000000078E-15, 0.9439899321577400748, 0.3299742535180970049 ) ) ;
#19618 = FACE_OUTER_BOUND ( 'NONE', #23768, .T. ) ;
#19619 = DIRECTION ( 'NONE',  ( -1.000000000000000000, 0.000000000000000000, 0.000000000000000000 ) ) ;
#19620 = CARTESIAN_POINT ( 'NONE',  ( 40.26954217208372455, -26.90384086642191619, 72.86986841596730358 ) ) ;
#19621 = LINE ( 'NONE', #12042, #15401 ) ;
#19622 = CARTESIAN_POINT ( 'NONE',  ( 37.61123632939165873, -1.913682088886106580, 73.73360434286902887 ) ) ;
#19623 = CYLINDRICAL_SURFACE ( 'NONE', #11857, 1.099999999999999645 ) ;
#19624 = AXIS2_PLACEMENT_3D ( 'NONE', #5954, #11763, #25117 ) ;
#19625 = ORIENTED_EDGE ( 'NONE', *, *, #20830, .T. ) ;
#19626 = EDGE_CURVE ( 'NONE', #16259, #4087, #13318, .T. ) ;
#19627 = EDGE_LOOP ( 'NONE', ( #11591, #21280, #17031, #4721 ) ) ;
#19628 = AXIS2_PLACEMENT_3D ( 'NONE', #7637, #13432, #7892 ) ;
#19629 = VECTOR ( 'NONE', #9083, 1000.000000000000000 ) ;
#19630 = CARTESIAN_POINT ( 'NONE',  ( 33.35284519649047752, 2.993954861727095906, 6.108562081104513375 ) ) ;
#19631 = EDGE_CURVE ( 'NONE', #5023, #13361, #20318, .T. ) ;
#19632 = FACE_OUTER_BOUND ( 'NONE', #12282, .T. ) ;
#19633 = CARTESIAN_POINT ( 'NONE',  ( 39.38009889167648936, -21.40384086642190553, 70.00779233799262613 ) ) ;
#19634 = EDGE_CURVE ( 'NONE', #2156, #14477, #18378, .T. ) ;
#19635 = DIRECTION ( 'NONE',  ( 0.000000000000000000, 0.000000000000000000, 1.000000000000000000 ) ) ;
#19636 = DIRECTION ( 'NONE',  ( 0.000000000000000000, 1.000000000000000000, 0.000000000000000000 ) ) ;
#19637 = ADVANCED_FACE ( 'NONE', ( #3664 ), #15269, .F. ) ;
#19638 = EDGE_CURVE ( 'NONE', #24147, #14083, #19259, .T. ) ;
#19639 = VERTEX_POINT ( 'NONE', #19016 ) ;
#19640 = DIRECTION ( 'NONE',  ( 2.412663730047098310E-15, -0.8967398287344625629, -0.4425581086832404143 ) ) ;
#19641 = CARTESIAN_POINT ( 'NONE',  ( 32.81606138205700773, 46.92314894770294131, 80.37823623207322044 ) ) ;
#19642 = CARTESIAN_POINT ( 'NONE',  ( 38.63098279924290068, -4.703840866421909794, 72.53360434286905445 ) ) ;
#19643 = ORIENTED_EDGE ( 'NONE', *, *, #10742, .F. ) ;
#19644 = EDGE_CURVE ( 'NONE', #467, #4421, #13468, .T. ) ;
#19645 = CARTESIAN_POINT ( 'NONE',  ( 31.56606138205708589, -42.63947656429714783, 70.74856838136764736 ) ) ;
#19646 = ORIENTED_EDGE ( 'NONE', *, *, #12267, .T. ) ;
#19647 = EDGE_LOOP ( 'NONE', ( #9106, #1198, #13751, #7565 ) ) ;
#19648 = VECTOR ( 'NONE', #9814, 1000.000000000000000 ) ;
#19649 = EDGE_CURVE ( 'NONE', #4383, #19118, #5606, .T. ) ;
#19650 = CARTESIAN_POINT ( 'NONE',  ( 33.66606138205698073, -7.467730535347549825, -2.778285769174305919 ) ) ;
#19651 = CARTESIAN_POINT ( 'NONE',  ( 37.31647492878122563, -11.31368208888609850, 70.72433947564853440 ) ) ;
#19652 = AXIS2_PLACEMENT_3D ( 'NONE', #22041, #6457, #20237 ) ;
#19653 = VECTOR ( 'NONE', #12747, 1000.000000000000000 ) ;
#19654 = CARTESIAN_POINT ( 'NONE',  ( 37.69225076346193504, -13.81368208888610383, 72.33091598616826445 ) ) ;
#19655 = ORIENTED_EDGE ( 'NONE', *, *, #3018, .F. ) ;
#19656 = VERTEX_POINT ( 'NONE', #7422 ) ;
#19657 = CARTESIAN_POINT ( 'NONE',  ( 47.84183937708599643, -33.05991196579839198, 70.24627502810386659 ) ) ;
#19658 = CARTESIAN_POINT ( 'NONE',  ( 36.81606138205700063, -4.070846987468769385, 59.14016975459033887 ) ) ;
#19659 = ORIENTED_EDGE ( 'NONE', *, *, #19649, .F. ) ;
#19660 = FACE_OUTER_BOUND ( 'NONE', #15119, .T. ) ;
#19661 = CARTESIAN_POINT ( 'NONE',  ( 39.82603832034400426, -15.30384086642190589, 70.35351908239857721 ) ) ;
#19662 = CARTESIAN_POINT ( 'NONE',  ( 36.32862050049384806, -20.56677809167894111, 75.94939806155714734 ) ) ;
#19663 = ADVANCED_FACE ( 'NONE', ( #13354 ), #7291, .T. ) ;
#19664 = LINE ( 'NONE', #20518, #5131 ) ;
#19665 = CARTESIAN_POINT ( 'NONE',  ( 39.51027997493896748, -16.51368208888610312, 71.32335560751960202 ) ) ;
#19666 = ORIENTED_EDGE ( 'NONE', *, *, #5647, .T. ) ;
#19667 = VERTEX_POINT ( 'NONE', #17590 ) ;
#19668 = DIRECTION ( 'NONE',  ( -3.373073425510455500E-16, -2.999999999999999839E-15, -1.000000000000000000 ) ) ;
#19669 = CARTESIAN_POINT ( 'NONE',  ( 36.87297107704153376, -13.71368208888610773, 72.49904802271740323 ) ) ;
#19670 = DIRECTION ( 'NONE',  ( -1.734723475976804876E-16, -3.491481338843135327E-15, -1.000000000000000000 ) ) ;
#19671 = LINE ( 'NONE', #7966, #15726 ) ;
#19672 = VECTOR ( 'NONE', #25282, 1000.000000000000000 ) ;
#19673 = AXIS2_PLACEMENT_3D ( 'NONE', #22108, #14136, #10020 ) ;
#19674 = DIRECTION ( 'NONE',  ( -1.301042606982603842E-16, 0.000000000000000000, -1.000000000000000000 ) ) ;
#19675 = FACE_OUTER_BOUND ( 'NONE', #17327, .T. ) ;
#19676 = ADVANCED_BREP_SHAPE_REPRESENTATION ( '', ( #17206, #2000 ), #20728 ) ;
#19677 = CARTESIAN_POINT ( 'NONE',  ( 34.81606138205696510, -1.975699482566735776, -4.057200616784870206 ) ) ;
#19678 = VERTEX_POINT ( 'NONE', #21079 ) ;
#19679 = PLANE ( 'NONE',  #14422 ) ;
#19680 = ORIENTED_EDGE ( 'NONE', *, *, #19349, .T. ) ;
#19681 = ORIENTED_EDGE ( 'NONE', *, *, #6906, .F. ) ;
#19682 = CARTESIAN_POINT ( 'NONE',  ( 39.64521430340305841, -4.803840866421917433, 73.30173637941818754 ) ) ;
#19683 = VERTEX_POINT ( 'NONE', #25033 ) ;
#19684 = CARTESIAN_POINT ( 'NONE',  ( 39.31606138205700063, 42.19123852234596939, 66.30501292736988717 ) ) ;
#19685 = CARTESIAN_POINT ( 'NONE',  ( 40.14115730948191185, -16.51368208888610667, 71.32335560751960202 ) ) ;
#19686 = VECTOR ( 'NONE', #17210, 1000.000000000000000 ) ;
#19687 = ORIENTED_EDGE ( 'NONE', *, *, #22004, .T. ) ;
#19688 = DIRECTION ( 'NONE',  ( 0.000000000000000000, 1.000000000000000000, -2.775557561562891351E-15 ) ) ;
#19689 = EDGE_CURVE ( 'NONE', #20356, #4383, #3420, .T. ) ;
#19690 = SURFACE_STYLE_FILL_AREA ( #24271 ) ;
#19691 = CARTESIAN_POINT ( 'NONE',  ( 37.61123632939165873, -15.91368208888610880, 73.73360434286898624 ) ) ;
#19692 = ADVANCED_FACE ( 'NONE', ( #11677 ), #21450, .F. ) ;
#19693 = AXIS2_PLACEMENT_3D ( 'NONE', #6308, #21634, #10048 ) ;
#19694 = DIRECTION ( 'NONE',  ( 9.027796614315171564E-31, 1.000000000000000000, 1.163336342344340343E-15 ) ) ;
#19695 = FACE_OUTER_BOUND ( 'NONE', #4470, .T. ) ;
#19696 = DIRECTION ( 'NONE',  ( -1.000000000000000000, -2.168404344971010101E-16, 1.734723475976814737E-16 ) ) ;
#19697 = DIRECTION ( 'NONE',  ( 0.000000000000000000, 0.6568589528324747517, -0.7540134720837718962 ) ) ;
#19698 = CARTESIAN_POINT ( 'NONE',  ( 42.06606138205700063, 43.19123852234599781, 74.30501292736987295 ) ) ;
#19699 = CARTESIAN_POINT ( 'NONE',  ( 37.89291511884479036, -12.50384086642191228, 72.49843995877330372 ) ) ;
#19700 = CARTESIAN_POINT ( 'NONE',  ( 38.63098279924288647, -28.91368208888610170, 70.22690120949089021 ) ) ;
#19701 = VECTOR ( 'NONE', #18350, 1000.000000000000000 ) ;
#19702 = ORIENTED_EDGE ( 'NONE', *, *, #10645, .F. ) ;
#19703 = CARTESIAN_POINT ( 'NONE',  ( 38.31606138205700063, -22.22127907754186893, 75.80501292736997243 ) ) ;
#19704 = FACE_OUTER_BOUND ( 'NONE', #4966, .T. ) ;
#19705 = ORIENTED_EDGE ( 'NONE', *, *, #19506, .T. ) ;
#19706 = VERTEX_POINT ( 'NONE', #1597 ) ;
#19707 = CARTESIAN_POINT ( 'NONE',  ( 40.55423172469004101, -23.20384086642191690, 70.70992431699450265 ) ) ;
#19708 = CIRCLE ( 'NONE', #1602, 2.000000000000001776 ) ;
#19709 = CARTESIAN_POINT ( 'NONE',  ( 37.31647492878122563, -25.31368208888610027, 70.72433947564853440 ) ) ;
#19710 = CARTESIAN_POINT ( 'NONE',  ( 38.26194895904383486, -1.013682088886101784, 69.04448340153881247 ) ) ;
#19711 = ORIENTED_EDGE ( 'NONE', *, *, #14823, .F. ) ;
#19712 = DIRECTION ( 'NONE',  ( -1.000000000000000000, 5.204170427930413997E-31, 1.734723475976804876E-16 ) ) ;
#19713 = EDGE_CURVE ( 'NONE', #8218, #12000, #19143, .T. ) ;
#19714 = CARTESIAN_POINT ( 'NONE',  ( 38.63098279924290068, -0.7038408664219106825, 72.53360434286905445 ) ) ;
#19715 = ADVANCED_FACE ( 'NONE', ( #11548 ), #13229, .F. ) ;
#19716 = DIRECTION ( 'NONE',  ( 8.673617379884039170E-17, 2.999999999999999839E-15, 1.000000000000000000 ) ) ;
#19717 = EDGE_LOOP ( 'NONE', ( #23873, #17476, #4790, #6094 ) ) ;
#19718 = CARTESIAN_POINT ( 'NONE',  ( 43.23147868389327897, 41.67000142393845152, 79.87823623207322044 ) ) ;
#19719 = EDGE_CURVE ( 'NONE', #1997, #8969, #22872, .T. ) ;
#19720 = DIRECTION ( 'NONE',  ( -4.812258323195720155E-32, 1.000000000000000000, -3.129456975819164530E-15 ) ) ;
#19721 = CARTESIAN_POINT ( 'NONE',  ( 40.55423172469004101, -1.203840866421914457, 70.70992431699450265 ) ) ;
#19722 = CARTESIAN_POINT ( 'NONE',  ( 40.31606138205700773, -4.357181138186127178, 82.80501292736992980 ) ) ;
#19723 = AXIS2_PLACEMENT_3D ( 'NONE', #4777, #10332, #16494 ) ;
#19724 = LINE ( 'NONE', #17418, #10361 ) ;
#19725 = CARTESIAN_POINT ( 'NONE',  ( 36.68196826583682935, -11.61368208888610276, 71.96809898377888715 ) ) ;
#19726 = DIRECTION ( 'NONE',  ( 3.469446951953614189E-15, -1.000000000000000000, 0.000000000000000000 ) ) ;
#19727 = LINE ( 'NONE', #514, #24141 ) ;
#19728 = AXIS2_PLACEMENT_3D ( 'NONE', #16281, #24127, #6504 ) ;
#19729 = CIRCLE ( 'NONE', #8635, 0.2314957320545540931 ) ;
#19730 = DIRECTION ( 'NONE',  ( 9.925461516413219746E-16, -0.8967398287344630070, -0.4425581086832393041 ) ) ;
#19731 = EDGE_CURVE ( 'NONE', #8890, #3872, #11416, .T. ) ;
#19732 = CARTESIAN_POINT ( 'NONE',  ( 37.25202387243754032, -2.403840866421914413, 72.75271321436733274 ) ) ;
#19733 = DIRECTION ( 'NONE',  ( 0.000000000000000000, 1.000000000000000000, -0.000000000000000000 ) ) ;
#19734 = AXIS2_PLACEMENT_3D ( 'NONE', #5489, #15142, #22997 ) ;
#19735 = CARTESIAN_POINT ( 'NONE',  ( 36.49096545463212493, -17.51368208888610667, 71.43714994484034264 ) ) ;
#19736 = CARTESIAN_POINT ( 'NONE',  ( 35.31606138205700773, 3.536347952325769040, 64.10938348997790115 ) ) ;
#19737 = CARTESIAN_POINT ( 'NONE',  ( 36.64852494920107517, -16.20384086642190979, 71.86517103874048473 ) ) ;
#19738 = CARTESIAN_POINT ( 'NONE',  ( 39.31606138205700063, 43.19123852234596939, 66.30501292736988717 ) ) ;
#19739 = VECTOR ( 'NONE', #16595, 1000.000000000000114 ) ;
#19740 = CARTESIAN_POINT ( 'NONE',  ( 40.14115730948191185, -14.51368208888610667, 71.32335560751960202 ) ) ;
#19741 = ORIENTED_EDGE ( 'NONE', *, *, #2404, .T. ) ;
#19742 = CARTESIAN_POINT ( 'NONE',  ( 35.86008812008917346, -19.51368208888610312, 71.43714994484034264 ) ) ;
#19743 = VERTEX_POINT ( 'NONE', #19385 ) ;
#19744 = LINE ( 'NONE', #15754, #4932 ) ;
#19745 = DIRECTION ( 'NONE',  ( 1.327674326049719602E-15, -0.4425581086832399147, 0.8967398287344627850 ) ) ;
#19746 = CARTESIAN_POINT ( 'NONE',  ( 39.31564783533279694, -19.30384086642191477, 70.72433947564853440 ) ) ;
#19747 = AXIS2_PLACEMENT_3D ( 'NONE', #6208, #21794, #4152 ) ;
#19748 = ORIENTED_EDGE ( 'NONE', *, *, #17774, .F. ) ;
#19749 = VECTOR ( 'NONE', #655, 1000.000000000000000 ) ;
#19750 = ORIENTED_EDGE ( 'NONE', *, *, #11473, .T. ) ;
#19751 = FACE_OUTER_BOUND ( 'NONE', #8098, .T. ) ;
#19752 = CARTESIAN_POINT ( 'NONE',  ( 40.31606138205700773, -10.93995761290683255, 80.99653337025984001 ) ) ;
#19753 = CARTESIAN_POINT ( 'NONE',  ( 39.95015449827720744, 0.9961591335780894951, 71.96809898377890136 ) ) ;
#19754 = VECTOR ( 'NONE', #21139, 1000.000000000000000 ) ;
#19755 = CARTESIAN_POINT ( 'NONE',  ( 32.81606138205700773, 18.19123852234598715, 71.05501292736995822 ) ) ;
#19756 = CARTESIAN_POINT ( 'NONE',  ( 37.50301148336529167, -5.113682088886100985, 69.06206559358666652 ) ) ;
#19757 = AXIS2_PLACEMENT_3D ( 'NONE', #16479, #253, #10574 ) ;
#19758 = FACE_OUTER_BOUND ( 'NONE', #14797, .T. ) ;
#19759 = ORIENTED_EDGE ( 'NONE', *, *, #24429, .T. ) ;
#19760 = ORIENTED_EDGE ( 'NONE', *, *, #20314, .F. ) ;
#19761 = CARTESIAN_POINT ( 'NONE',  ( 35.81606138205700063, 5.191238522346999673, 69.30501292736998664 ) ) ;
#19762 = CARTESIAN_POINT ( 'NONE',  ( 38.38987944808049235, -39.60718113818700203, 84.30501292737011454 ) ) ;
#19763 = EDGE_CURVE ( 'NONE', #23326, #16761, #330, .T. ) ;
#19764 = CARTESIAN_POINT ( 'NONE',  ( 36.49096545463212493, -24.10384086642190482, 71.32335560751960202 ) ) ;
#19765 =( NAMED_UNIT ( * ) PLANE_ANGLE_UNIT ( ) SI_UNIT ( $, .RADIAN. ) );
#19766 = DIRECTION ( 'NONE',  ( 1.000000000000000000, 0.000000000000000000, 0.000000000000000000 ) ) ;
#19767 = ORIENTED_EDGE ( 'NONE', *, *, #19104, .F. ) ;
#19768 = VECTOR ( 'NONE', #8154, 1000.000000000000114 ) ;
#19769 = DIRECTION ( 'NONE',  ( -1.000000000000000078E-15, 0.9439899321577400748, 0.3299742535180970049 ) ) ;
#19770 = CIRCLE ( 'NONE', #18135, 1.750000000000001554 ) ;
#19771 = LINE ( 'NONE', #11930, #23823 ) ;
#19772 = ORIENTED_EDGE ( 'NONE', *, *, #20895, .T. ) ;
#19773 = CARTESIAN_POINT ( 'NONE',  ( 39.02742774030101458, -9.403840866421907307, 70.49320253461759478 ) ) ;
#19774 = LINE ( 'NONE', #1630, #13568 ) ;
#19775 = EDGE_LOOP ( 'NONE', ( #12334, #23423, #13332, #1893 ) ) ;
#19776 = DIRECTION ( 'NONE',  ( 0.000000000000000000, -0.7540134720837717852, -0.6568589528324745297 ) ) ;
#19777 = ORIENTED_EDGE ( 'NONE', *, *, #8562, .F. ) ;
#19778 = ORIENTED_EDGE ( 'NONE', *, *, #10136, .F. ) ;
#19779 = DIRECTION ( 'NONE',  ( 1.000000000000000000, 2.999999999999999839E-15, 0.000000000000000000 ) ) ;
#19780 = UNCERTAINTY_MEASURE_WITH_UNIT (LENGTH_MEASURE( 1.000000000000000082E-05 ), #6888, 'distance_accuracy_value', 'NONE');
#19781 = CARTESIAN_POINT ( 'NONE',  ( 37.31647492878122563, -13.31368208888610205, 70.72433947564853440 ) ) ;
#19782 = EDGE_CURVE ( 'NONE', #16417, #2969, #7549, .T. ) ;
#19783 = CARTESIAN_POINT ( 'NONE',  ( 37.31647492878122563, -3.313682088886101607, 70.72433947564853440 ) ) ;
#19784 = VERTEX_POINT ( 'NONE', #23245 ) ;
#19785 = ORIENTED_EDGE ( 'NONE', *, *, #4532, .T. ) ;
#19786 = DIRECTION ( 'NONE',  ( 0.000000000000000000, 1.000000000000000000, -3.469446951953614189E-15 ) ) ;
#19787 = CARTESIAN_POINT ( 'NONE',  ( 43.31606138205700063, 7.535758204303438568, 66.26723409915207696 ) ) ;
#19788 = ORIENTED_EDGE ( 'NONE', *, *, #20592, .T. ) ;
#19789 = DIRECTION ( 'NONE',  ( 0.000000000000000000, -0.8212051873014252212, -0.5706330172266858014 ) ) ;
#19790 = CARTESIAN_POINT ( 'NONE',  ( 38.37017380507018771, -15.60384086642190837, 69.64448340153877837 ) ) ;
#19791 = EDGE_CURVE ( 'NONE', #3043, #24906, #18046, .T. ) ;
#19792 = AXIS2_PLACEMENT_3D ( 'NONE', #5749, #21844, #65 ) ;
#19793 = DIRECTION ( 'NONE',  ( -2.727049986597864201E-15, 0.7516416929448760387, 0.6595716529892418079 ) ) ;
#19794 = DIRECTION ( 'NONE',  ( 1.000000000000000000, -0.000000000000000000, 0.000000000000000000 ) ) ;
#19795 = CARTESIAN_POINT ( 'NONE',  ( 39.24876120206128860, -18.71368208888610241, 70.63227792289245599 ) ) ;
#19796 = ORIENTED_EDGE ( 'NONE', *, *, #1189, .T. ) ;
#19797 = CIRCLE ( 'NONE', #862, 2.000000000000000000 ) ;
#19798 = ORIENTED_EDGE ( 'NONE', *, *, #5702, .F. ) ;
#19799 = CARTESIAN_POINT ( 'NONE',  ( 40.81606138205700773, 37.44123852234599781, 75.30501292736990138 ) ) ;
#19800 = CARTESIAN_POINT ( 'NONE',  ( 37.80618814713140097, -11.91368208888611058, 73.13360434286903455 ) ) ;
#19801 = EDGE_CURVE ( 'NONE', #15157, #13632, #15516, .T. ) ;
#19802 = DIRECTION ( 'NONE',  ( 0.000000000000000000, -1.000000000000000000, 2.999999999999999839E-15 ) ) ;
#19803 = CARTESIAN_POINT ( 'NONE',  ( 34.56606138205700773, 45.04446929126255128, 81.37823623207320622 ) ) ;
#19804 = DIRECTION ( 'NONE',  ( 0.000000000000000000, 0.7540134720837717852, 0.6568589528324746407 ) ) ;
#19805 = CARTESIAN_POINT ( 'NONE',  ( 40.16586900051838427, -29.10876147765365829, 71.27221389253728034 ) ) ;
#19806 = PRODUCT ( 'Pusher Pull Spring', 'Pusher Pull Spring', '', ( #5695 ) ) ;
#19807 = CARTESIAN_POINT ( 'NONE',  ( 32.31606138205700063, -20.93319939328399926, 43.78741072286599945 ) ) ;
#19808 = CARTESIAN_POINT ( 'NONE',  ( 29.81606138205706458, -34.55876147768187678, 70.30501292735635843 ) ) ;
#19809 = VERTEX_POINT ( 'NONE', #23368 ) ;
#19810 = CARTESIAN_POINT ( 'NONE',  ( 36.72059563575756158, -21.43489111338284658, 75.33538682622121030 ) ) ;
#19811 = ORIENTED_EDGE ( 'NONE', *, *, #6322, .T. ) ;
#19812 = ORIENTED_EDGE ( 'NONE', *, *, #19132, .F. ) ;
#19813 = PRESENTATION_LAYER_ASSIGNMENT (  '', '', ( #16505 ) ) ;
#19814 = CARTESIAN_POINT ( 'NONE',  ( 40.33642880535521869, -7.303840866421912104, 69.98269868914867686 ) ) ;
#19815 = EDGE_CURVE ( 'NONE', #15268, #8846, #17089, .T. ) ;
#19816 = ORIENTED_EDGE ( 'NONE', *, *, #9562, .T. ) ;
#19817 = AXIS2_PLACEMENT_3D ( 'NONE', #22062, #23859, #4426 ) ;
#19818 = DIRECTION ( 'NONE',  ( -3.491481338843135327E-15, -1.000000000000000000, 2.999999999999999839E-15 ) ) ;
#19819 = CARTESIAN_POINT ( 'NONE',  ( 38.93415946300897446, -8.113682088886108090, 73.09843995877331224 ) ) ;
#19820 = EDGE_CURVE ( 'NONE', #5864, #12889, #6117, .T. ) ;
#19821 = EDGE_CURVE ( 'NONE', #10110, #10123, #765, .T. ) ;
#19822 = ORIENTED_EDGE ( 'NONE', *, *, #8560, .F. ) ;
#19823 = DIRECTION ( 'NONE',  ( 1.000000000000000000, 2.751104698760144965E-15, -1.228345504986737969E-16 ) ) ;
#19824 = CARTESIAN_POINT ( 'NONE',  ( 40.52078840805428683, -14.61368208888610276, 70.60699637195608602 ) ) ;
#19825 = CARTESIAN_POINT ( 'NONE',  ( 43.81606138205700063, 18.19123852234599070, 72.05501292736995822 ) ) ;
#19826 = DIRECTION ( 'NONE',  ( 0.000000000000000000, 0.5706330172266952383, -0.8212051873014186709 ) ) ;
#19827 = ADVANCED_FACE ( 'NONE', ( #2241 ), #7802, .F. ) ;
#19828 = VECTOR ( 'NONE', #17128, 1000.000000000000000 ) ;
#19829 = CARTESIAN_POINT ( 'NONE',  ( 35.56606138205703616, -24.72749677399389157, 32.19456755146972426 ) ) ;
#19830 = PLANE ( 'NONE',  #24208 ) ;
#19831 = VECTOR ( 'NONE', #18513, 1000.000000000000000 ) ;
#19832 = CARTESIAN_POINT ( 'NONE',  ( 34.81606138205696510, -1.316127829577488528, -4.808842309729777220 ) ) ;
#19833 = CARTESIAN_POINT ( 'NONE',  ( 33.31606138205700773, -5.204193249396280585, 82.80501292736992980 ) ) ;
#19834 = CARTESIAN_POINT ( 'NONE',  ( 39.51027997493896748, -26.51368208888610667, 71.32335560751960202 ) ) ;
#19835 = ORIENTED_EDGE ( 'NONE', *, *, #19791, .F. ) ;
#19836 = DIRECTION ( 'NONE',  ( -2.412663730047099099E-15, 0.8967398287344627850, 0.4425581086832399147 ) ) ;
#19837 = EDGE_CURVE ( 'NONE', #3712, #3791, #23635, .T. ) ;
#19838 = CARTESIAN_POINT ( 'NONE',  ( 44.81606138205700063, 40.34464305740947765, 81.44836866983821722 ) ) ;
#19839 = VERTEX_POINT ( 'NONE', #23875 ) ;
#19840 = ORIENTED_EDGE ( 'NONE', *, *, #9662, .F. ) ;
#19841 = CARTESIAN_POINT ( 'NONE',  ( 39.12911128074872380, -25.50384086642191406, 69.06206559358663810 ) ) ;
#19842 = CARTESIAN_POINT ( 'NONE',  ( 37.21915885897815457, -21.41368208888610525, 71.08074471024443142 ) ) ;
#19843 = CARTESIAN_POINT ( 'NONE',  ( 38.93415946300897446, -28.11368208888610098, 73.09843995877328382 ) ) ;
#19844 = DIRECTION ( 'NONE',  ( -1.000000000000000000, 0.000000000000000000, 0.000000000000000000 ) ) ;
#19845 = VECTOR ( 'NONE', #1908, 1000.000000000000000 ) ;
#19846 = CARTESIAN_POINT ( 'NONE',  ( 39.24876120206129571, -0.9038408664219128585, 72.12822762946750288 ) ) ;
#19847 = DIRECTION ( 'NONE',  ( -1.734723475976809806E-16, 0.000000000000000000, -1.000000000000000000 ) ) ;
#19848 = VERTEX_POINT ( 'NONE', #21701 ) ;
#19849 = CARTESIAN_POINT ( 'NONE',  ( 40.81606138205700773, 37.44123852234599781, 75.30501292736990138 ) ) ;
#19850 = CARTESIAN_POINT ( 'NONE',  ( 43.81606138205700063, -34.55876147765401640, 70.30501292737011454 ) ) ;
#19851 = AXIS2_PLACEMENT_3D ( 'NONE', #317, #24264, #14369 ) ;
#19852 = CARTESIAN_POINT ( 'NONE',  ( 37.50301148336529877, -4.503840866421918498, 73.69843995877330656 ) ) ;
#19853 = CARTESIAN_POINT ( 'NONE',  ( 45.81606138205700063, -34.55876147765410167, 70.30501292737000085 ) ) ;
#19854 = CARTESIAN_POINT ( 'NONE',  ( 33.24019963865212191, 3.104051971978903701, 6.135536383744724098 ) ) ;
#19855 = CARTESIAN_POINT ( 'NONE',  ( 36.68196826583682935, -9.613682088886104538, 71.96809898377890136 ) ) ;
#19856 = LINE ( 'NONE', #4400, #3961 ) ;
#19857 = AXIS2_PLACEMENT_3D ( 'NONE', #10043, #8366, #6304 ) ;
#19858 = VECTOR ( 'NONE', #2666, 1000.000000000000000 ) ;
#19859 = CARTESIAN_POINT ( 'NONE',  ( 36.49096545463212493, -25.51368208888610312, 71.43714994484031422 ) ) ;
#19860 = LINE ( 'NONE', #2202, #23033 ) ;
#19861 = CARTESIAN_POINT ( 'NONE',  ( 38.37017380507018771, 0.3961591335780931256, 69.64448340153880679 ) ) ;
#19862 = AXIS2_PLACEMENT_3D ( 'NONE', #11160, #16430, #18625 ) ;
#19863 = EDGE_CURVE ( 'NONE', #24395, #15753, #299, .T. ) ;
#19864 = DIRECTION ( 'NONE',  ( 0.000000000000000000, 3.469446951953611033E-15, 1.000000000000000000 ) ) ;
#19865 = CARTESIAN_POINT ( 'NONE',  ( 37.89291511884479036, -24.50384086642190695, 72.49843995877328950 ) ) ;
#19866 = CARTESIAN_POINT ( 'NONE',  ( 36.87297107704152666, -9.713682088886107735, 72.49904802271743165 ) ) ;
#19867 = ADVANCED_FACE ( 'NONE', ( #2487 ), #424, .T. ) ;
#19868 = CARTESIAN_POINT ( 'NONE',  ( 33.31606138205700773, -16.48551471403133206, 77.11349248448009064 ) ) ;
#19869 = ADVANCED_FACE ( 'NONE', ( #8056 ), #21956, .T. ) ;
#19870 = VECTOR ( 'NONE', #16769, 1000.000000000000000 ) ;
#19871 = CARTESIAN_POINT ( 'NONE',  ( 39.75915168707251723, -14.90384086642191086, 72.49904802271738902 ) ) ;
#19872 = DIRECTION ( 'NONE',  ( 0.000000000000000000, 1.000000000000000000, -2.999999999999999839E-15 ) ) ;
#19873 = AXIS2_PLACEMENT_3D ( 'NONE', #21986, #4213, #22106 ) ;
#19874 = CARTESIAN_POINT ( 'NONE',  ( 37.69796330110504101, -15.11368208888609743, 69.66206559358661821 ) ) ;
#19875 = EDGE_LOOP ( 'NONE', ( #1778, #6143, #5089, #21623 ) ) ;
#19876 = CARTESIAN_POINT ( 'NONE',  ( 36.89935272106204422, -17.21368208888610241, 69.52238214136768590 ) ) ;
#19877 = ORIENTED_EDGE ( 'NONE', *, *, #6858, .T. ) ;
#19878 = CARTESIAN_POINT ( 'NONE',  ( 40.81606138205700063, 5.191238522346999673, 69.30501292736998664 ) ) ;
#19879 = CARTESIAN_POINT ( 'NONE',  ( 33.80827534892208064, -20.02093502212017029, 26.61211107664843212 ) ) ;
#19880 = CARTESIAN_POINT ( 'NONE',  ( 38.00113996487112189, -19.70384086642190979, 70.22690120949090442 ) ) ;
#19881 = VERTEX_POINT ( 'NONE', #4056 ) ;
#19882 = ORIENTED_EDGE ( 'NONE', *, *, #17366, .T. ) ;
#19883 = PLANE ( 'NONE',  #9659 ) ;
#19884 = EDGE_CURVE ( 'NONE', #3466, #16707, #10116, .T. ) ;
#19885 = CARTESIAN_POINT ( 'NONE',  ( 32.81606138205700773, 2.191238522347000117, 69.30501292737000085 ) ) ;
#19886 = VECTOR ( 'NONE', #3770, 1000.000000000000227 ) ;
#19887 = CARTESIAN_POINT ( 'NONE',  ( 35.86008812008917346, -20.10384086642191548, 71.32335560751961623 ) ) ;
#19888 = AXIS2_PLACEMENT_3D ( 'NONE', #5447, #1321, #1449 ) ;
#19889 = DIRECTION ( 'NONE',  ( -9.925461516413221718E-16, 0.8967398287344632291, 0.4425581086832394151 ) ) ;
#19890 = CARTESIAN_POINT ( 'NONE',  ( 37.69796330110504101, -27.11368208888609388, 69.66206559358660400 ) ) ;
#19891 = AXIS2_PLACEMENT_3D ( 'NONE', #24988, #5684, #9440 ) ;
#19892 = CARTESIAN_POINT ( 'NONE',  ( 43.81606138205700063, 34.92314894770294131, 81.17823623207323180 ) ) ;
#19893 = ORIENTED_EDGE ( 'NONE', *, *, #7052, .F. ) ;
#19894 = ORIENTED_EDGE ( 'NONE', *, *, #15336, .T. ) ;
#19895 = LINE ( 'NONE', #2234, #6326 ) ;
#19896 = CARTESIAN_POINT ( 'NONE',  ( 33.31606138205700773, -16.48551471403133206, 77.11349248448009064 ) ) ;
#19897 = VECTOR ( 'NONE', #19253, 1000.000000000000227 ) ;
#19898 = CARTESIAN_POINT ( 'NONE',  ( 36.49096545463212493, -22.10384086642191193, 71.32335560751961623 ) ) ;
#19899 = FILL_AREA_STYLE ('',( #21824 ) ) ;
#19900 = CARTESIAN_POINT ( 'NONE',  ( 29.81606138205707524, -38.13418765192407989, 68.51141129791366780 ) ) ;
#19901 = EDGE_LOOP ( 'NONE', ( #4107, #13411 ) ) ;
#19902 = DIRECTION ( 'NONE',  ( 9.999999999999998805E-16, -0.9439899321577399638, -0.3299742535180969494 ) ) ;
#19903 = AXIS2_PLACEMENT_3D ( 'NONE', #1527, #13404, #13282 ) ;
#19904 = CARTESIAN_POINT ( 'NONE',  ( 33.31606138205700773, -20.88462213363798270, 44.49284693533410717 ) ) ;
#19905 = CARTESIAN_POINT ( 'NONE',  ( 39.24876120206129571, -2.903840866421911304, 72.12822762946750288 ) ) ;
#19906 = FACE_OUTER_BOUND ( 'NONE', #6115, .T. ) ;
#19907 = ORIENTED_EDGE ( 'NONE', *, *, #16312, .F. ) ;
#19908 = AXIS2_PLACEMENT_3D ( 'NONE', #5154, #16876, #18936 ) ;
#19909 = PLANE ( 'NONE',  #15673 ) ;
#19910 = ORIENTED_EDGE ( 'NONE', *, *, #17141, .F. ) ;
#19911 = VERTEX_POINT ( 'NONE', #14233 ) ;
#19912 = LINE ( 'NONE', #23885, #14384 ) ;
#19913 = CARTESIAN_POINT ( 'NONE',  ( 44.81606138205700063, -26.74044063519535186, 82.50501292737007475 ) ) ;
#19914 = CARTESIAN_POINT ( 'NONE',  ( 37.12184278917507640, -7.513682088886100452, 71.43714994484035685 ) ) ;
#19915 = CARTESIAN_POINT ( 'NONE',  ( 38.93987200065208754, -2.813682088886101162, 70.42958956619168021 ) ) ;
#19916 = ORIENTED_EDGE ( 'NONE', *, *, #12714, .T. ) ;
#19917 = ORIENTED_EDGE ( 'NONE', *, *, #14948, .F. ) ;
#19918 = CARTESIAN_POINT ( 'NONE',  ( 33.40064408022072939, 41.90149715599300606, 79.87823623207322044 ) ) ;
#19919 = ADVANCED_FACE ( 'NONE', ( #2361 ), #11928, .T. ) ;
#19920 = DIRECTION ( 'NONE',  ( 0.000000000000000000, 0.000000000000000000, -1.000000000000000000 ) ) ;
#19921 = DIRECTION ( 'NONE',  ( 0.000000000000000000, -0.5706330172266919076, 0.8212051873014208914 ) ) ;
#19922 = CARTESIAN_POINT ( 'NONE',  ( 37.33957961208645315, -7.803840866421909439, 69.94417936956673998 ) ) ;
#19923 = STYLED_ITEM ( 'NONE', ( #11298 ), #9253 ) ;
#19924 = DIRECTION ( 'NONE',  ( 7.071067811865491110E-16, -0.9008287146801832179, 0.4341746501209495790 ) ) ;
#19925 = CYLINDRICAL_SURFACE ( 'NONE', #10573, 0.5000000000000004441 ) ;
#19926 = ORIENTED_EDGE ( 'NONE', *, *, #23565, .T. ) ;
#19927 = CIRCLE ( 'NONE', #3474, 1.000000000000000888 ) ;
#19928 = AXIS2_PLACEMENT_3D ( 'NONE', #11825, #6738, #21727 ) ;
#19929 = ORIENTED_EDGE ( 'NONE', *, *, #4044, .T. ) ;
#19930 = DIRECTION ( 'NONE',  ( 1.327674326049719602E-15, -0.4425581086832399147, 0.8967398287344627850 ) ) ;
#19931 = CARTESIAN_POINT ( 'NONE',  ( 39.75915168707250302, -8.713682088886098853, 70.26145752964255564 ) ) ;
#19932 = LINE ( 'NONE', #459, #19246 ) ;
#19933 = CARTESIAN_POINT ( 'NONE',  ( 31.81606138205700418, 28.69846577177642288, 66.12638289304319983 ) ) ;
#19934 = DIRECTION ( 'NONE',  ( 1.000000000000000000, 0.000000000000000000, 0.000000000000000000 ) ) ;
#19935 = CARTESIAN_POINT ( 'NONE',  ( 40.20245935045282692, -29.10876147765143429, 71.09018146340289945 ) ) ;
#19936 = CARTESIAN_POINT ( 'NONE',  ( 33.31606138205700773, 3.172506336381830661, 12.50058896911730066 ) ) ;
#19937 = DIRECTION ( 'NONE',  ( 1.000000000000000000, 2.554104467024131702E-15, 1.134076704137112863E-15 ) ) ;
#19938 = PRODUCT_DEFINITION_FORMATION_WITH_SPECIFIED_SOURCE ( 'ANY', '', #17752, .NOT_KNOWN. ) ;
#19939 = LINE ( 'NONE', #16064, #11161 ) ;
#19940 = VERTEX_POINT ( 'NONE', #9988 ) ;
#19941 = ORIENTED_EDGE ( 'NONE', *, *, #8500, .F. ) ;
#19942 = AXIS2_PLACEMENT_3D ( 'NONE', #10605, #8678, #16510 ) ;
#19943 = PLANE ( 'NONE',  #21891 ) ;
#19944 = CARTESIAN_POINT ( 'NONE',  ( 36.29569395875881099, -2.303840866421917877, 72.77780686321129622 ) ) ;
#19945 = ORIENTED_EDGE ( 'NONE', *, *, #20664, .F. ) ;
#19946 = EDGE_CURVE ( 'NONE', #8440, #947, #5865, .T. ) ;
#19947 = CARTESIAN_POINT ( 'NONE',  ( 44.81606138205700063, 40.39281886181299797, 80.75501292736983316 ) ) ;
#19948 = CARTESIAN_POINT ( 'NONE',  ( 36.64852494920107517, -9.413682088886107024, 70.89533451361948835 ) ) ;
#19949 = AXIS2_PLACEMENT_3D ( 'NONE', #3180, #6930, #6803 ) ;
#19950 = ORIENTED_EDGE ( 'NONE', *, *, #4557, .T. ) ;
#19951 = DIRECTION ( 'NONE',  ( 1.734723475976814737E-16, -1.000000000000000000, 3.491481338843135327E-15 ) ) ;
#19952 = CARTESIAN_POINT ( 'NONE',  ( 36.07789103942398867, -15.41368208888610347, 70.70992431699450265 ) ) ;
#19953 = CARTESIAN_POINT ( 'NONE',  ( 43.13775064171697693, 2.905199411292878953, 6.099582584402872598 ) ) ;
#19954 = CARTESIAN_POINT ( 'NONE',  ( 43.81606138205700063, -37.34243788671330577, 70.80615726751818784 ) ) ;
#19955 = ORIENTED_EDGE ( 'NONE', *, *, #14374, .F. ) ;
#19956 = AXIS2_PLACEMENT_3D ( 'NONE', #9156, #20741, #3077 ) ;
#19957 = CYLINDRICAL_SURFACE ( 'NONE', #5856, 1.500000000000001332 ) ;
#19958 = EDGE_CURVE ( 'NONE', #19015, #1986, #22076, .T. ) ;
#19959 = EDGE_CURVE ( 'NONE', #9905, #10647, #15897, .T. ) ;
#19960 = CARTESIAN_POINT ( 'NONE',  ( 43.81606138205700063, -21.31259689655800216, 45.10875082581016926 ) ) ;
#19961 = EDGE_CURVE ( 'NONE', #10371, #24890, #178, .T. ) ;
#19962 = CARTESIAN_POINT ( 'NONE',  ( 43.05893433410182070, 3.408565912792066221, 6.350990188909392486 ) ) ;
#19963 = ADVANCED_FACE ( 'NONE', ( #23999 ), #25417, .T. ) ;
#19964 = DIRECTION ( 'NONE',  ( 0.000000000000000000, 2.999999999999999839E-15, 1.000000000000000000 ) ) ;
#19965 = CARTESIAN_POINT ( 'NONE',  ( 37.38336156205274818, -25.71368208888610241, 72.12822762946747446 ) ) ;
#19966 = EDGE_CURVE ( 'NONE', #18865, #17790, #15778, .T. ) ;
#19967 = ORIENTED_EDGE ( 'NONE', *, *, #1376, .T. ) ;
#19968 = CARTESIAN_POINT ( 'NONE',  ( 38.83707137437546919, -22.15989686853476925, 75.80517981147842477 ) ) ;
#19969 = LINE ( 'NONE', #8630, #11983 ) ;
#19970 = ORIENTED_EDGE ( 'NONE', *, *, #16732, .T. ) ;
#19971 = ORIENTED_EDGE ( 'NONE', *, *, #3670, .F. ) ;
#19972 = CARTESIAN_POINT ( 'NONE',  ( 37.61123632939164452, -23.70384086642191335, 69.02690120949091579 ) ) ;
#19973 = EDGE_CURVE ( 'NONE', #15276, #3312, #4186, .T. ) ;
#19974 = CARTESIAN_POINT ( 'NONE',  ( 38.26194895904383486, 0.9863179111139001032, 69.04448340153882668 ) ) ;
#19975 = CARTESIAN_POINT ( 'NONE',  ( 36.31606138205700773, -20.93502329652820038, 27.89939821807130826 ) ) ;
#19976 = VECTOR ( 'NONE', #21627, 1000.000000000000000 ) ;
#19977 = EDGE_CURVE ( 'NONE', #1424, #4665, #6617, .T. ) ;
#19978 = DIRECTION ( 'NONE',  ( 1.000000000000000000, 0.000000000000000000, 0.000000000000000000 ) ) ;
#19979 = ORIENTED_EDGE ( 'NONE', *, *, #19313, .T. ) ;
#19980 = DIRECTION ( 'NONE',  ( 0.000000000000000000, -0.5706330172266952383, 0.8212051873014186709 ) ) ;
#19981 = CARTESIAN_POINT ( 'NONE',  ( 36.06606138205697931, -5.948051402551132405, 9.959574150503843981 ) ) ;
#19982 = CARTESIAN_POINT ( 'NONE',  ( 38.26194895904384197, -4.603840866421918143, 73.71602215082116061 ) ) ;
#19983 = FACE_OUTER_BOUND ( 'NONE', #12403, .T. ) ;
#19984 = DIRECTION ( 'NONE',  ( -1.734723475976809806E-16, 1.000000000000000000, -3.269436733918100469E-15 ) ) ;
#19985 = CARTESIAN_POINT ( 'NONE',  ( 38.26194895904383486, -9.013682088886101340, 69.64448340153879258 ) ) ;
#19986 = CARTESIAN_POINT ( 'NONE',  ( 28.81606138205698286, -4.589472609077256848, -6.350807634294814541 ) ) ;
#19987 = CARTESIAN_POINT ( 'NONE',  ( 39.38009889167650357, -24.21368208888610596, 72.75271321436730432 ) ) ;
#19988 = DIRECTION ( 'NONE',  ( 1.000000000000000000, -5.204170427930415223E-30, -1.734723475976805122E-15 ) ) ;
#19989 = CARTESIAN_POINT ( 'NONE',  ( 39.95015449827720744, -1.003840866421912281, 71.96809898377888715 ) ) ;
#19990 = DIRECTION ( 'NONE',  ( 1.000000000000000000, -1.301042606982604506E-30, -4.336808689942015271E-16 ) ) ;
#19991 = CARTESIAN_POINT ( 'NONE',  ( 38.63098279924290068, -24.70384086642190979, 72.53360434286901182 ) ) ;
#19992 = CARTESIAN_POINT ( 'NONE',  ( 36.68196826583682935, -11.61368208888610276, 71.96809898377888715 ) ) ;
#19993 = DIRECTION ( 'NONE',  ( 1.000000000000000000, 0.000000000000000000, 0.000000000000000000 ) ) ;
#19994 = CARTESIAN_POINT ( 'NONE',  ( 39.82603832034400426, -11.30384086642190944, 70.35351908239857721 ) ) ;
#19995 = CARTESIAN_POINT ( 'NONE',  ( 38.31606138205700063, 12.69123852234700678, 71.30501292736997243 ) ) ;
#19996 = CARTESIAN_POINT ( 'NONE',  ( 37.80618814713140097, -9.913682088886107024, 73.13360434286904876 ) ) ;
#19997 = ORIENTED_EDGE ( 'NONE', *, *, #625, .F. ) ;
#19998 = CARTESIAN_POINT ( 'NONE',  ( 36.11133435605973574, -15.61368208888610454, 72.15350918040385864 ) ) ;
#19999 = VERTEX_POINT ( 'NONE', #20400 ) ;
#20000 = CARTESIAN_POINT ( 'NONE',  ( 30.81606138205696510, -0.7562224151693580643, -1.633662118351544734 ) ) ;
#20001 = FACE_OUTER_BOUND ( 'NONE', #25433, .T. ) ;
#20002 = CARTESIAN_POINT ( 'NONE',  ( 38.93987200065210175, -16.80384086642191477, 72.33091598616826445 ) ) ;
#20003 = ORIENTED_EDGE ( 'NONE', *, *, #5341, .T. ) ;
#20004 = VERTEX_POINT ( 'NONE', #2994 ) ;
#20005 = DIRECTION ( 'NONE',  ( -1.000000000000000000, 6.018531076210110289E-31, 1.734723475976804876E-16 ) ) ;
#20006 = CARTESIAN_POINT ( 'NONE',  ( 40.31606138205700773, -16.48551471403133206, 77.11349248448009064 ) ) ;
#20007 = CARTESIAN_POINT ( 'NONE',  ( 37.50301148336529877, -20.50384086642191761, 73.69843995877327814 ) ) ;
#20008 = B_SPLINE_CURVE_WITH_KNOTS ( 'NONE', 3,
 ( #20037, #16415, #18489, #22223, #22092, #2877 ),
 .UNSPECIFIED., .F., .F.,
 ( 4, 2, 4 ),
 ( 0.000000000000000000, 0.5000000000000000000, 1.000000000000000000 ),
 .UNSPECIFIED. ) ;
#20009 = DIRECTION ( 'NONE',  ( 1.000000000000000000, 1.187136597504755470E-16, 8.249087426255173666E-17 ) ) ;
#20010 = CARTESIAN_POINT ( 'NONE',  ( 38.82593461698262871, -26.91368208888610170, 69.62690120949091011 ) ) ;
#20011 = PRODUCT_RELATED_PRODUCT_CATEGORY ( 'part', '', ( #23697 ) ) ;
#20012 = PRODUCT_DEFINITION_SHAPE ( 'NONE', 'NONE',  #25493 ) ;
#20013 = CARTESIAN_POINT ( 'NONE',  ( 40.81606138205700773, -24.05876147765399864, 75.30501292737008612 ) ) ;
#20014 = EDGE_CURVE ( 'NONE', #17850, #3732, #23391, .T. ) ;
#20015 = ORIENTED_EDGE ( 'NONE', *, *, #15109, .F. ) ;
#20016 = ORIENTED_EDGE ( 'NONE', *, *, #8801, .T. ) ;
#20017 = CARTESIAN_POINT ( 'NONE',  ( 33.23689862680489426, 3.100967383408606448, 6.133394271278472587 ) ) ;
#20018 = PLANE ( 'NONE',  #14679 ) ;
#20019 = CARTESIAN_POINT ( 'NONE',  ( 39.75915168707251723, -18.90384086642191264, 72.49904802271738902 ) ) ;
#20020 = SURFACE_SIDE_STYLE ('',( #5991 ) ) ;
#20021 = DIRECTION ( 'NONE',  ( 0.000000000000000000, 1.000000000000000000, -2.999999999999999839E-15 ) ) ;
#20022 = ORIENTED_EDGE ( 'NONE', *, *, #10523, .T. ) ;
#20023 = CARTESIAN_POINT ( 'NONE',  ( 32.81606138205700773, 46.92314894770294131, 80.37823623207322044 ) ) ;
#20024 = DIRECTION ( 'NONE',  ( 2.792262043613788535E-15, -0.8967398287344627850, -0.4425581086832399147 ) ) ;
#20025 = CARTESIAN_POINT ( 'NONE',  ( 37.69225076346193504, 0.1961591335780874246, 70.42958956619168021 ) ) ;
#20026 = CARTESIAN_POINT ( 'NONE',  ( 43.31606138205700063, -33.70281195181703993, 69.07320514641659770 ) ) ;
#20027 = ORIENTED_EDGE ( 'NONE', *, *, #18033, .F. ) ;
#20028 = CARTESIAN_POINT ( 'NONE',  ( 38.31606138205700063, -22.22127907754186893, 75.80501292736997243 ) ) ;
#20029 = ORIENTED_EDGE ( 'NONE', *, *, #5176, .F. ) ;
#20030 = ORIENTED_EDGE ( 'NONE', *, *, #554, .T. ) ;
#20031 = LINE ( 'NONE', #10248, #23434 ) ;
#20032 = CARTESIAN_POINT ( 'NONE',  ( 29.81606138205696155, -0.7562224151693598406, -1.633662118351544734 ) ) ;
#20033 = CARTESIAN_POINT ( 'NONE',  ( 37.69225076346193504, -7.813682088886102939, 72.33091598616827866 ) ) ;
#20034 = CARTESIAN_POINT ( 'NONE',  ( 38.00113996487114321, -1.913682088886099475, 72.53360434286905445 ) ) ;
#20035 = VERTEX_POINT ( 'NONE', #10751 ) ;
#20036 = ORIENTED_EDGE ( 'NONE', *, *, #8636, .T. ) ;
#20037 = CARTESIAN_POINT ( 'NONE',  ( 33.31606138205700773, 4.124002793203064066, 6.312068993173404863 ) ) ;
#20038 = LINE ( 'NONE', #16416, #13278 ) ;
#20039 = ORIENTED_EDGE ( 'NONE', *, *, #9826, .T. ) ;
#20040 = DIRECTION ( 'NONE',  ( 0.000000000000000000, 1.000000000000000000, 0.000000000000000000 ) ) ;
#20041 = CARTESIAN_POINT ( 'NONE',  ( 36.64852494920107517, -12.20384086642190979, 71.86517103874048473 ) ) ;
#20042 = CIRCLE ( 'NONE', #23718, 12.59999999999999964 ) ;
#20043 = EDGE_CURVE ( 'NONE', #13011, #3712, #5314, .T. ) ;
#20044 = EDGE_CURVE ( 'NONE', #12956, #10061, #11482, .T. ) ;
#20045 = VECTOR ( 'NONE', #9984, 1000.000000000000000 ) ;
#20046 = CIRCLE ( 'NONE', #13461, 9.500000000000001776 ) ;
#20047 = DIRECTION ( 'NONE',  ( 0.000000000000000000, 0.6595716529892415858, -0.7516416929448760387 ) ) ;
#20048 = FACE_OUTER_BOUND ( 'NONE', #13955, .T. ) ;
#20049 = EDGE_LOOP ( 'NONE', ( #12847, #15458, #11556, #21206 ) ) ;
#20050 = ORIENTED_EDGE ( 'NONE', *, *, #22810, .T. ) ;
#20051 = ORIENTED_EDGE ( 'NONE', *, *, #3502, .T. ) ;
#20052 = DIRECTION ( 'NONE',  ( 0.000000000000000000, 1.000000000000000000, 0.000000000000000000 ) ) ;
#20053 = CARTESIAN_POINT ( 'NONE',  ( 36.80608444377001121, -7.313682088886101162, 70.35351908239861984 ) ) ;
#20054 = LINE ( 'NONE', #328, #10616 ) ;
#20055 = FACE_BOUND ( 'NONE', #25167, .T. ) ;
#20056 = CARTESIAN_POINT ( 'NONE',  ( 40.31606138205700773, -7.204193249396275256, 83.11277699141410835 ) ) ;
#20057 = CARTESIAN_POINT ( 'NONE',  ( 40.31606138205700773, -11.51539968388051705, 18.41550321377400934 ) ) ;
#20058 = EDGE_CURVE ( 'NONE', #194, #131, #22168, .T. ) ;
#20059 = VECTOR ( 'NONE', #1044, 1000.000000000000000 ) ;
#20060 = DIRECTION ( 'NONE',  ( 1.000000000000000000, -0.000000000000000000, 0.000000000000000000 ) ) ;
#20061 = DIRECTION ( 'NONE',  ( 0.000000000000000000, -3.965082230804126670E-15, -1.000000000000000000 ) ) ;
#20062 = VECTOR ( 'NONE', #20113, 1000.000000000000227 ) ;
#20063 = VECTOR ( 'NONE', #23666, 1000.000000000000114 ) ;
#20064 = CARTESIAN_POINT ( 'NONE',  ( 36.80477597196090045, -21.53774254971854418, 75.32796878085879655 ) ) ;
#20065 = ORIENTED_EDGE ( 'NONE', *, *, #18912, .T. ) ;
#20066 = ORIENTED_EDGE ( 'NONE', *, *, #5941, .F. ) ;
#20067 = CARTESIAN_POINT ( 'NONE',  ( 44.81606138205700063, -34.55876147765400930, 73.30501292737011454 ) ) ;
#20068 = CARTESIAN_POINT ( 'NONE',  ( 39.02088643472237806, -4.703840866421917788, 73.73360434286902887 ) ) ;
#20069 = ORIENTED_EDGE ( 'NONE', *, *, #24177, .F. ) ;
#20070 = CARTESIAN_POINT ( 'NONE',  ( 40.31606138205700773, -22.22127907754180853, 85.30501292736998664 ) ) ;
#20071 = CARTESIAN_POINT ( 'NONE',  ( 39.98359781491296161, -10.41368208888610347, 71.86517103874048473 ) ) ;
#20072 = CARTESIAN_POINT ( 'NONE',  ( 43.31606138205700063, 3.043703737701412226, 64.67489359404071081 ) ) ;
#20073 = CARTESIAN_POINT ( 'NONE',  ( 37.50301148336529167, -17.11368208888609743, 69.06206559358665231 ) ) ;
#20074 = AXIS2_PLACEMENT_3D ( 'NONE', #12635, #10820, #12888 ) ;
#20075 = CARTESIAN_POINT ( 'NONE',  ( 41.06606138205703616, -24.72749677399387735, 32.19456755146972426 ) ) ;
#20076 = AXIS2_PLACEMENT_3D ( 'NONE', #1709, #11538, #5855 ) ;
#20077 = AXIS2_PLACEMENT_3D ( 'NONE', #14633, #16820, #7030 ) ;
#20078 = CARTESIAN_POINT ( 'NONE',  ( 40.31606138205700063, 8.691238522346997897, 68.80501292736998664 ) ) ;
#20079 = DIRECTION ( 'NONE',  ( -1.000000000000000000, 0.000000000000000000, 0.000000000000000000 ) ) ;
#20080 = CARTESIAN_POINT ( 'NONE',  ( 35.64099152588522657, 0.3928188618129990761, 80.05501292736997243 ) ) ;
#20081 = EDGE_CURVE ( 'NONE', #7071, #10377, #8943, .T. ) ;
#20082 = DIRECTION ( 'NONE',  ( -1.000000000000000000, 0.000000000000000000, 0.000000000000000000 ) ) ;
#20083 = DIRECTION ( 'NONE',  ( 0.000000000000000000, 1.000000000000000000, -2.999999999999999839E-15 ) ) ;
#20084 = CARTESIAN_POINT ( 'NONE',  ( 37.60469502381300089, -25.21368208888610241, 70.49320253461758057 ) ) ;
#20085 = VERTEX_POINT ( 'NONE', #4571 ) ;
#20086 = LINE ( 'NONE', #20467, #19739 ) ;
#20087 = DIRECTION ( 'NONE',  ( 1.000000000000000000, 0.000000000000000000, 0.000000000000000000 ) ) ;
#20088 = EDGE_LOOP ( 'NONE', ( #1611, #14255, #5986, #12784 ) ) ;
#20089 = EDGE_LOOP ( 'NONE', ( #14828, #16959, #19643, #14392 ) ) ;
#20090 = UNCERTAINTY_MEASURE_WITH_UNIT (LENGTH_MEASURE( 1.000000000000000082E-05 ), #6048, 'distance_accuracy_value', 'NONE');
#20091 = CARTESIAN_POINT ( 'NONE',  ( 40.77203464402485622, -23.10384086642191548, 71.43714994484032843 ) ) ;
#20092 = TOROIDAL_SURFACE ( 'NONE', #16799, 0.2314957320545545372, 0.5000000000000000000 ) ;
#20093 = CARTESIAN_POINT ( 'NONE',  ( 36.64852494920107517, -25.41368208888610525, 70.89533451361945993 ) ) ;
#20094 = DIRECTION ( 'NONE',  ( 3.717264591378870232E-16, 3.115648231731786715E-15, 1.000000000000000000 ) ) ;
#20095 = AXIS2_PLACEMENT_3D ( 'NONE', #15318, #7724, #11596 ) ;
#20096 = EDGE_CURVE ( 'NONE', #3821, #1971, #2861, .T. ) ;
#20098 = EDGE_CURVE ( 'NONE', #11457, #5208, #12438, .T. ) ;
#20097 = CARTESIAN_POINT ( 'NONE',  ( 32.81606138205700773, -36.11063010576116739, 71.66210679335823386 ) ) ;
#20099 = EDGE_LOOP ( 'NONE', ( #4908, #7577, #8335, #3437, #8701, #11028, #6160 ) ) ;
#20100 = CARTESIAN_POINT ( 'NONE',  ( 38.82716350840370723, -5.250869752214502917, 82.80533778410890022 ) ) ;
#20101 = FACE_OUTER_BOUND ( 'NONE', #7146, .T. ) ;
#20102 = CARTESIAN_POINT ( 'NONE',  ( 39.02088643472237806, -6.703840866421919564, 73.73360434286902887 ) ) ;
#20103 = EDGE_CURVE ( 'NONE', #21012, #8428, #16664, .T. ) ;
#20104 = EDGE_CURVE ( 'NONE', #4547, #14366, #24494, .T. ) ;
#20105 = AXIS2_PLACEMENT_3D ( 'NONE', #5847, #2563, #4515 ) ;
#20106 = EDGE_CURVE ( 'NONE', #15148, #8601, #10496, .T. ) ;
#20107 = CARTESIAN_POINT ( 'NONE',  ( 43.81608638205700146, 2.887189827768484207, 12.91119156276801228 ) ) ;
#20108 = CARTESIAN_POINT ( 'NONE',  ( 35.81606138205700063, 5.691238522347000561, 69.30501292736998664 ) ) ;
#20109 = CARTESIAN_POINT ( 'NONE',  ( 37.33957961208646736, -5.813682088886107380, 72.81632618279323310 ) ) ;
#20110 = CARTESIAN_POINT ( 'NONE',  ( 32.56606138205700773, 43.35512946304240245, 81.37823623207322044 ) ) ;
#20111 = CARTESIAN_POINT ( 'NONE',  ( 39.95015449827720744, -28.61368208888610454, 70.79240656858104330 ) ) ;
#20112 = VECTOR ( 'NONE', #9740, 1000.000000000000000 ) ;
#20113 = DIRECTION ( 'NONE',  ( 0.000000000000000000, 0.9814242980364923374, 0.1918498038142812112 ) ) ;
#20114 = EDGE_CURVE ( 'NONE', #9377, #16043, #932, .T. ) ;
#20115 = CARTESIAN_POINT ( 'NONE',  ( 45.81606138205705037, -30.46100403034031245, 72.05704881431053366 ) ) ;
#20116 = CARTESIAN_POINT ( 'NONE',  ( 43.18074167159075216, 3.582118287471805385, 6.336670741225087333 ) ) ;
#20117 = CARTESIAN_POINT ( 'NONE',  ( 38.73920764526923932, -25.50384086642191406, 70.26206559358661252 ) ) ;
#20118 = CARTESIAN_POINT ( 'NONE',  ( 38.93415946300897446, -12.11368208888610276, 73.09843995877329803 ) ) ;
#20119 = CARTESIAN_POINT ( 'NONE',  ( 33.31606138205700773, 3.536347952325769040, 64.10938348997790115 ) ) ;
#20120 = AXIS2_PLACEMENT_3D ( 'NONE', #1294, #24857, #7102 ) ;
#20121 = CARTESIAN_POINT ( 'NONE',  ( 37.33957961208645315, -11.80384086642190944, 69.94417936956672577 ) ) ;
#20122 = DIRECTION ( 'NONE',  ( -1.000000000000000000, -3.091505625455828697E-15, -4.515976121274772923E-17 ) ) ;
#20123 = CARTESIAN_POINT ( 'NONE',  ( 39.29254315202756231, -10.81368208888610205, 69.94417936956673998 ) ) ;
#20124 = ORIENTED_EDGE ( 'NONE', *, *, #8960, .F. ) ;
#20125 = CARTESIAN_POINT ( 'NONE',  ( 37.61123632939165873, -17.91368208888610525, 73.73360434286898624 ) ) ;
#20126 = ORIENTED_EDGE ( 'NONE', *, *, #666, .F. ) ;
#20127 = CARTESIAN_POINT ( 'NONE',  ( 45.81606138205700063, -11.72563467517899838, 72.98595903681223263 ) ) ;
#20128 = LINE ( 'NONE', #159, #2178 ) ;
#20129 = CIRCLE ( 'NONE', #356, 0.7500000000000008882 ) ;
#20130 = CARTESIAN_POINT ( 'NONE',  ( 38.00113996487112189, -17.70384086642190979, 70.22690120949090442 ) ) ;
#20131 = VECTOR ( 'NONE', #6344, 1000.000000000000000 ) ;
#20132 = ORIENTED_EDGE ( 'NONE', *, *, #16436, .F. ) ;
#20133 = ORIENTED_EDGE ( 'NONE', *, *, #16265, .T. ) ;
#20134 = CARTESIAN_POINT ( 'NONE',  ( 42.68042513965293949, 15.19123852234700323, 70.30501292736995822 ) ) ;
#20135 = LINE ( 'NONE', #16005, #3428 ) ;
#20136 = CARTESIAN_POINT ( 'NONE',  ( 35.86008812008917346, -24.10384086642191193, 71.32335560751960202 ) ) ;
#20137 = ADVANCED_FACE ( 'NONE', ( #10622 ), #6749, .T. ) ;
#20138 = VECTOR ( 'NONE', #23292, 1000.000000000000114 ) ;
#20139 = ADVANCED_FACE ( 'NONE', ( #8823 ), #14851, .F. ) ;
#20140 = LINE ( 'NONE', #24108, #7189 ) ;
#20141 = CARTESIAN_POINT ( 'NONE',  ( 39.95015449827720744, -28.61368208888610454, 70.79240656858104330 ) ) ;
#20142 = LINE ( 'NONE', #2230, #18842 ) ;
#20143 = AXIS2_PLACEMENT_3D ( 'NONE', #7586, #17630, #11582 ) ;
#20144 = ORIENTED_EDGE ( 'NONE', *, *, #24193, .F. ) ;
#20145 = VECTOR ( 'NONE', #6173, 1000.000000000000000 ) ;
#20146 = DIRECTION ( 'NONE',  ( 2.341661252633485168E-15, -0.7516416929448815898, -0.6595716529892353686 ) ) ;
#20147 = CARTESIAN_POINT ( 'NONE',  ( 38.09940268710882094, 37.69123852234599781, 70.07393250355386272 ) ) ;
#20148 = EDGE_CURVE ( 'NONE', #20521, #952, #22334, .T. ) ;
#20149 = CARTESIAN_POINT ( 'NONE',  ( 36.87297107704151244, -13.90384086642190731, 70.26145752964255564 ) ) ;
#20150 = CARTESIAN_POINT ( 'NONE',  ( 38.31606138205712853, 43.19123852234599781, 75.30501292736987295 ) ) ;
#20151 = AXIS2_PLACEMENT_3D ( 'NONE', #6556, #20347, #14418 ) ;
#20152 = DIRECTION ( 'NONE',  ( 6.195440985631459015E-17, 1.000000000000000000, -2.999999999999999839E-15 ) ) ;
#20153 = LINE ( 'NONE', #11802, #11966 ) ;
#20154 = CARTESIAN_POINT ( 'NONE',  ( 39.31564783533279694, -1.303840866421910105, 70.72433947564853440 ) ) ;
#20155 = AXIS2_PLACEMENT_3D ( 'NONE', #11041, #18898, #4581 ) ;
#20156 = CARTESIAN_POINT ( 'NONE',  ( 43.31606138205700063, -12.40281258615395465, 20.95421293576468358 ) ) ;
#20157 = ORIENTED_EDGE ( 'NONE', *, *, #15398, .T. ) ;
#20158 = EDGE_CURVE ( 'NONE', #6977, #14863, #14725, .T. ) ;
#20159 = CARTESIAN_POINT ( 'NONE',  ( 38.37017380507020192, -28.01368208888610667, 73.11602215082115208 ) ) ;
#20160 = ORIENTED_EDGE ( 'NONE', *, *, #22134, .F. ) ;
#20161 = ORIENTED_EDGE ( 'NONE', *, *, #21086, .F. ) ;
#20162 = DIRECTION ( 'NONE',  ( 0.000000000000000000, 0.4425581086832397482, -0.8967398287344628960 ) ) ;
#20163 = CARTESIAN_POINT ( 'NONE',  ( 43.23147868389327897, 41.43850569188389699, 79.37823623207322044 ) ) ;
#20164 = CARTESIAN_POINT ( 'NONE',  ( 39.41296390513587511, -6.413682088886100807, 71.67976084211552745 ) ) ;
#20165 = CARTESIAN_POINT ( 'NONE',  ( 37.12184278917507640, -7.513682088886100452, 71.43714994484035685 ) ) ;
#20166 = VERTEX_POINT ( 'NONE', #20527 ) ;
#20167 = ORIENTED_EDGE ( 'NONE', *, *, #13046, .T. ) ;
#20168 = CARTESIAN_POINT ( 'NONE',  ( 30.81606138205700418, 46.92314894770294131, 81.17823623207320338 ) ) ;
#20169 = CARTESIAN_POINT ( 'NONE',  ( 36.31606138205700063, -7.204193249396275256, 83.11277699141410835 ) ) ;
#20170 = ORIENTED_EDGE ( 'NONE', *, *, #16974, .F. ) ;
#20171 = DIRECTION ( 'NONE',  ( 0.000000000000000000, -1.000000000000000000, 0.000000000000000000 ) ) ;
#20172 = CARTESIAN_POINT ( 'NONE',  ( 37.69796330110505522, -12.50384086642191228, 73.09843995877329803 ) ) ;
#20173 = CARTESIAN_POINT ( 'NONE',  ( 40.31606138205700773, -30.30876147765400574, 73.55501292737010033 ) ) ;
#20174 = CARTESIAN_POINT ( 'NONE',  ( 30.81606138205700418, 0.1601050959395486362, 68.80395113470939350 ) ) ;
#20175 = VERTEX_POINT ( 'NONE', #6870 ) ;
#20176 = VERTEX_POINT ( 'NONE', #22586 ) ;
#20177 = VERTEX_POINT ( 'NONE', #6494 ) ;
#20178 = PLANE ( 'NONE',  #13720 ) ;
#20179 = VECTOR ( 'NONE', #22276, 1000.000000000000000 ) ;
#20180 = CARTESIAN_POINT ( 'NONE',  ( 39.29254315202756231, -8.813682088886100274, 69.94417936956673998 ) ) ;
#20181 = EDGE_LOOP ( 'NONE', ( #21300, #8419, #13396, #8454 ) ) ;
#20182 = LINE ( 'NONE', #4216, #13901 ) ;
#20183 = DIRECTION ( 'NONE',  ( 1.000000000000000000, 3.066740595113354287E-15, 9.534026549497653239E-17 ) ) ;
#20184 = CIRCLE ( 'NONE', #9090, 0.7500000000000006661 ) ;
#20185 = CARTESIAN_POINT ( 'NONE',  ( 38.93415946300897446, -26.11368208888610098, 73.09843995877328382 ) ) ;
#20186 = DIRECTION ( 'NONE',  ( -2.442401846778130416E-15, 0.8967398287344627850, 0.4425581086832399147 ) ) ;
#20187 = EDGE_CURVE ( 'NONE', #13086, #10846, #14478, .T. ) ;
#20188 = DIRECTION ( 'NONE',  ( -2.048868001712896742E-15, 0.6595716529892345914, -0.7516416929448823669 ) ) ;
#20189 = DIRECTION ( 'NONE',  ( 1.000000000000000000, 0.000000000000000000, -0.000000000000000000 ) ) ;
#20190 = EDGE_CURVE ( 'NONE', #6145, #7242, #15578, .T. ) ;
#20191 = EDGE_CURVE ( 'NONE', #20177, #13483, #9457, .T. ) ;
#20192 = DIRECTION ( 'NONE',  ( 0.000000000000000000, -0.6595716529892415858, 0.7516416929448761497 ) ) ;
#20193 = EDGE_LOOP ( 'NONE', ( #4344, #20702, #689, #21056 ) ) ;
#20194 = VERTEX_POINT ( 'NONE', #15360 ) ;
#20195 = CARTESIAN_POINT ( 'NONE',  ( 41.31606138205700063, 3.195231713396695650, 64.80689721350518084 ) ) ;
#20196 = CARTESIAN_POINT ( 'NONE',  ( 35.86008812008917346, -2.103840866421915923, 71.32335560751961623 ) ) ;
#20197 = CIRCLE ( 'NONE', #15239, 1.000000000000000888 ) ;
#20198 = ORIENTED_EDGE ( 'NONE', *, *, #12598, .F. ) ;
#20199 = ORIENTED_EDGE ( 'NONE', *, *, #23489, .F. ) ;
#20200 = CARTESIAN_POINT ( 'NONE',  ( 38.14273442609844977, 40.69123852234599781, 70.32014858831708182 ) ) ;
#20201 = CARTESIAN_POINT ( 'NONE',  ( 36.80608444377001121, -11.31368208888609672, 70.35351908239857721 ) ) ;
#20202 = VECTOR ( 'NONE', #21204, 1000.000000000000000 ) ;
#20203 = CYLINDRICAL_SURFACE ( 'NONE', #5054, 10.00000000000000000 ) ;
#20204 = EDGE_CURVE ( 'NONE', #24906, #20256, #5701, .T. ) ;
#20205 = CARTESIAN_POINT ( 'NONE',  ( 40.33642880535524000, -16.31368208888611093, 72.77780686321126780 ) ) ;
#20206 = DIRECTION ( 'NONE',  ( 0.000000000000000000, 1.000000000000000000, 0.000000000000000000 ) ) ;
#20207 = DIRECTION ( 'NONE',  ( -1.000000000000000000, 0.000000000000000000, 0.000000000000000000 ) ) ;
#20208 = CARTESIAN_POINT ( 'NONE',  ( 40.31606138205700773, 43.19123852234599781, 75.30501292736987295 ) ) ;
#20209 = SURFACE_STYLE_USAGE ( .BOTH. , #12235 ) ;
#20210 = DIRECTION ( 'NONE',  ( -0.000000000000000000, -1.000000000000000000, 2.848211695852029218E-15 ) ) ;
#20211 = DIRECTION ( 'NONE',  ( -1.000000000000000000, 0.000000000000000000, 0.000000000000000000 ) ) ;
#20212 = AXIS2_PLACEMENT_3D ( 'NONE', #8455, #4460, #20171 ) ;
#20213 = CARTESIAN_POINT ( 'NONE',  ( 31.81606138205700418, -33.05876147765410167, 70.30501292737000085 ) ) ;
#20214 = CARTESIAN_POINT ( 'NONE',  ( 38.26194895904383486, -25.01368208888610312, 70.24448340153875847 ) ) ;
#20215 = VERTEX_POINT ( 'NONE', #15108 ) ;
#20216 = CARTESIAN_POINT ( 'NONE',  ( 40.11656585159207822, -21.10173941565100009, 75.36713447021789136 ) ) ;
#20217 = DIRECTION ( 'NONE',  ( -1.000000000000000000, 0.000000000000000000, 0.000000000000000000 ) ) ;
#20218 = ORIENTED_EDGE ( 'NONE', *, *, #18672, .F. ) ;
#20219 = ORIENTED_EDGE ( 'NONE', *, *, #24646, .F. ) ;
#20220 = CARTESIAN_POINT ( 'NONE',  ( 36.29569395875881099, -24.30384086642192187, 72.77780686321126780 ) ) ;
#20221 = CARTESIAN_POINT ( 'NONE',  ( 38.37017380507020192, 1.986317911113890666, 73.71602215082117482 ) ) ;
#20222 = CARTESIAN_POINT ( 'NONE',  ( 43.31606138205700773, -19.13113579875041381, 24.60350147050422720 ) ) ;
#20223 = DIRECTION ( 'NONE',  ( 1.000000000000000000, 2.751104698760144965E-15, -1.228345504986737969E-16 ) ) ;
#20224 = SURFACE_STYLE_USAGE ( .BOTH. , #13831 ) ;
#20225 = VERTEX_POINT ( 'NONE', #17058 ) ;
#20226 = LINE ( 'NONE', #2565, #12157 ) ;
#20227 = CARTESIAN_POINT ( 'NONE',  ( 32.81606138205700773, 41.44123852234596939, 66.30501292736988717 ) ) ;
#20228 = EDGE_CURVE ( 'NONE', #10110, #2757, #4882, .T. ) ;
#20229 = CARTESIAN_POINT ( 'NONE',  ( 40.77203464402485622, -5.103840866421915479, 71.43714994484034264 ) ) ;
#20230 = AXIS2_PLACEMENT_3D ( 'NONE', #4362, #6295, #16576 ) ;
#20231 = CARTESIAN_POINT ( 'NONE',  ( 33.31606138205700773, -20.88462213363798270, 44.49284693533410717 ) ) ;
#20232 = DIRECTION ( 'NONE',  ( 0.000000000000000000, 0.5706330172266907974, -0.8212051873014217795 ) ) ;
#20233 = CARTESIAN_POINT ( 'NONE',  ( 36.49096545463212493, -9.513682088886101340, 71.43714994484035685 ) ) ;
#20234 = CARTESIAN_POINT ( 'NONE',  ( 45.61606138205700489, 44.92314894770294131, 81.37823623207322044 ) ) ;
#20235 = MECHANICAL_DESIGN_GEOMETRIC_PRESENTATION_REPRESENTATION (  '', ( #9146 ), #23518 ) ;
#20236 = CARTESIAN_POINT ( 'NONE',  ( 37.80618814713140097, -25.91368208888610880, 73.13360434286902034 ) ) ;
#20237 = DIRECTION ( 'NONE',  ( 0.000000000000000000, 1.000000000000000000, 0.000000000000000000 ) ) ;
#20238 = CARTESIAN_POINT ( 'NONE',  ( 38.41621794735363693, -36.60729675983900222, 84.30501292737011454 ) ) ;
#20239 = CARTESIAN_POINT ( 'NONE',  ( 39.24876120206129571, -26.90384086642191264, 72.12822762946746025 ) ) ;
#20240 = CARTESIAN_POINT ( 'NONE',  ( 38.37017380507020192, -14.01368208888610845, 73.11602215082116629 ) ) ;
#20241 = ORIENTED_EDGE ( 'NONE', *, *, #6176, .F. ) ;
#20242 = CARTESIAN_POINT ( 'NONE',  ( 38.31606138205700063, -29.37462871496113337, 53.20604314849776983 ) ) ;
#20243 = AXIS2_PLACEMENT_3D ( 'NONE', #17613, #25317, #25443 ) ;
#20244 = ORIENTED_EDGE ( 'NONE', *, *, #17518, .F. ) ;
#20245 = VECTOR ( 'NONE', #16206, 1000.000000000000000 ) ;
#20246 = CARTESIAN_POINT ( 'NONE',  ( 39.29254315202757653, -14.80384086642191477, 72.81632618279321889 ) ) ;
#20247 = FACE_OUTER_BOUND ( 'NONE', #7139, .T. ) ;
#20248 = VECTOR ( 'NONE', #6290, 1000.000000000000227 ) ;
#20249 = CARTESIAN_POINT ( 'NONE',  ( 39.38009889167650357, -4.213682088886106847, 72.75271321436733274 ) ) ;
#20250 = ORIENTED_EDGE ( 'NONE', *, *, #23549, .F. ) ;
#20251 = CARTESIAN_POINT ( 'NONE',  ( 40.55423172469004811, -18.41368208888610525, 72.05058123536544201 ) ) ;
#20252 = VERTEX_POINT ( 'NONE', #23211 ) ;
#20253 = DIRECTION ( 'NONE',  ( 0.000000000000000000, 0.7540134720837717852, 0.6568589528324746407 ) ) ;
#20254 = FACE_OUTER_BOUND ( 'NONE', #15277, .T. ) ;
#20255 = CARTESIAN_POINT ( 'NONE',  ( 38.37017380507018771, -15.60384086642191370, 70.24448340153875847 ) ) ;
#20256 = VERTEX_POINT ( 'NONE', #22966 ) ;
#20257 = ORIENTED_EDGE ( 'NONE', *, *, #17120, .T. ) ;
#20258 = AXIS2_PLACEMENT_3D ( 'NONE', #15700, #21128, #21632 ) ;
#20259 = DIRECTION ( 'NONE',  ( -0.000000000000000000, -3.469446951953613400E-15, -1.000000000000000000 ) ) ;
#20260 = LINE ( 'NONE', #19885, #17005 ) ;
#20261 = EDGE_CURVE ( 'NONE', #9779, #8969, #25261, .T. ) ;
#20262 = CARTESIAN_POINT ( 'NONE',  ( 38.37017380507018771, -21.60384086642191548, 69.04448340153878405 ) ) ;
#20263 = FACE_OUTER_BOUND ( 'NONE', #16644, .T. ) ;
#20264 = CARTESIAN_POINT ( 'NONE',  ( 39.98359781491296161, -26.41368208888610525, 71.86517103874045631 ) ) ;
#20265 = DIRECTION ( 'NONE',  ( 1.000000000000000000, 2.168404344971055214E-16, -1.734723475976814737E-16 ) ) ;
#20266 = DIRECTION ( 'NONE',  ( 0.000000000000000000, 2.999999999999999839E-15, 1.000000000000000000 ) ) ;
#20267 = AXIS2_PLACEMENT_3D ( 'NONE', #11675, #21075, #21447 ) ;
#20268 = ADVANCED_BREP_SHAPE_REPRESENTATION ( '', ( #25265, #2000 ), #17482 ) ;
#20269 = ORIENTED_EDGE ( 'NONE', *, *, #16116, .T. ) ;
#20270 = CARTESIAN_POINT ( 'NONE',  ( 34.06606138205700773, -33.77966242919868733, 58.66916295099436951 ) ) ;
#20271 = CARTESIAN_POINT ( 'NONE',  ( 44.81606138205700063, -24.55876147765401285, 70.30501292737008612 ) ) ;
#20272 = VECTOR ( 'NONE', #24017, 1000.000000000000000 ) ;
#20273 = CARTESIAN_POINT ( 'NONE',  ( 37.80618814713138676, -13.70384086642190802, 69.62690120949091011 ) ) ;
#20274 = DIRECTION ( 'NONE',  ( 0.000000000000000000, 0.000000000000000000, 1.000000000000000000 ) ) ;
#20275 = CYLINDRICAL_SURFACE ( 'NONE', #20715, 2.000000000000000888 ) ;
#20276 = EDGE_CURVE ( 'NONE', #23854, #19348, #13192, .T. ) ;
#20277 = VERTEX_POINT ( 'NONE', #3630 ) ;
#20278 = ADVANCED_FACE ( 'NONE', ( #21043 ), #19227, .T. ) ;
#20279 = CARTESIAN_POINT ( 'NONE',  ( 43.81606138205700063, -36.55876147765401640, 71.30501292737011454 ) ) ;
#20280 = AXIS2_PLACEMENT_3D ( 'NONE', #6644, #16689, #4839 ) ;
#20281 = CIRCLE ( 'NONE', #12879, 0.5000000000000036637 ) ;
#20282 = CARTESIAN_POINT ( 'NONE',  ( 39.48763425731081611, -21.82678658219787948, 29.70634659473178374 ) ) ;
#20283 = EDGE_CURVE ( 'NONE', #6369, #3058, #7391, .T. ) ;
#20284 = CARTESIAN_POINT ( 'NONE',  ( 38.37017380507018771, -1.603840866421912148, 70.24448340153877268 ) ) ;
#20285 = ADVANCED_FACE ( 'NONE', ( #21289 ), #1689, .T. ) ;
#20286 = CARTESIAN_POINT ( 'NONE',  ( 38.18494427818247061, -22.22127907754186893, 75.80501292736997243 ) ) ;
#20287 = VERTEX_POINT ( 'NONE', #20916 ) ;
#20288 = VECTOR ( 'NONE', #15624, 1000.000000000000000 ) ;
#20289 = DIRECTION ( 'NONE',  ( 0.000000000000000000, -3.469446951953613400E-15, -1.000000000000000000 ) ) ;
#20290 = ORIENTED_EDGE ( 'NONE', *, *, #6950, .F. ) ;
#20291 = ORIENTED_EDGE ( 'NONE', *, *, #12616, .F. ) ;
#20292 = CARTESIAN_POINT ( 'NONE',  ( 36.52316816324354676, 8.484131741160446438, 65.30501292736998664 ) ) ;
#20293 = VECTOR ( 'NONE', #8210, 1000.000000000000000 ) ;
#20294 = CARTESIAN_POINT ( 'NONE',  ( 40.81606138205700063, 5.191238522346999673, 69.30501292736998664 ) ) ;
#20295 = CARTESIAN_POINT ( 'NONE',  ( 38.00113996487114321, -5.913682088886099919, 72.53360434286905445 ) ) ;
#20296 = CARTESIAN_POINT ( 'NONE',  ( 37.21915885897815457, -3.413682088886101251, 71.08074471024443142 ) ) ;
#20297 = ORIENTED_EDGE ( 'NONE', *, *, #18346, .F. ) ;
#20298 = EDGE_LOOP ( 'NONE', ( #4822, #20022, #5336, #22930 ) ) ;
#20299 = CARTESIAN_POINT ( 'NONE',  ( 28.81606138205697931, -31.26685248843966747, 43.18544225915084667 ) ) ;
#20300 = VECTOR ( 'NONE', #14086, 1000.000000000000000 ) ;
#20301 = DIRECTION ( 'NONE',  ( -2.048868001712899108E-15, 0.6595716529892353686, -0.7516416929448815898 ) ) ;
#20302 = EDGE_CURVE ( 'NONE', #2134, #10314, #1191, .T. ) ;
#20303 = CARTESIAN_POINT ( 'NONE',  ( 31.56606138205697576, -5.918777154956194053, -5.916875169744970187 ) ) ;
#20304 = CARTESIAN_POINT ( 'NONE',  ( 36.80608444377001831, -8.303840866421916544, 72.40698646996136745 ) ) ;
#20305 = EDGE_CURVE ( 'NONE', #24159, #14544, #7643, .T. ) ;
#20306 =( NAMED_UNIT ( * ) SI_UNIT ( $, .STERADIAN. ) SOLID_ANGLE_UNIT ( ) );
#20307 = AXIS2_PLACEMENT_3D ( 'NONE', #12933, #12561, #18465 ) ;
#20308 = LINE ( 'NONE', #23777, #1926 ) ;
#20309 = ORIENTED_EDGE ( 'NONE', *, *, #8147, .T. ) ;
#20310 = EDGE_LOOP ( 'NONE', ( #11562, #5011, #23496, #21743 ) ) ;
#20311 = VERTEX_POINT ( 'NONE', #1452 ) ;
#20312 = LINE ( 'NONE', #22736, #2172 ) ;
#20313 = CARTESIAN_POINT ( 'NONE',  ( 39.38009889167650357, -6.213682088886108623, 72.75271321436733274 ) ) ;
#20314 = EDGE_CURVE ( 'NONE', #10213, #9175, #7258, .T. ) ;
#20315 = CARTESIAN_POINT ( 'NONE',  ( 39.78769017101468108, -29.10876147765122823, 70.98199272578698071 ) ) ;
#20316 = VECTOR ( 'NONE', #11512, 1000.000000000000000 ) ;
#20317 = DIRECTION ( 'NONE',  ( 0.000000000000000000, -2.999999999999999839E-15, -1.000000000000000000 ) ) ;
#20318 = LINE ( 'NONE', #18505, #7761 ) ;
#20319 = AXIS2_PLACEMENT_3D ( 'NONE', #19850, #12140, #10189 ) ;
#20320 = DIRECTION ( 'NONE',  ( 1.123589211228918605E-15, -0.4425581086832399147, 0.8967398287344627850 ) ) ;
#20321 = CYLINDRICAL_SURFACE ( 'NONE', #22956, 1.500000000000000222 ) ;
#20322 = VECTOR ( 'NONE', #7253, 1000.000000000000000 ) ;
#20323 = CARTESIAN_POINT ( 'NONE',  ( 36.36526940127878760, -20.73543518430840749, 75.41293983993888617 ) ) ;
#20324 = VERTEX_POINT ( 'NONE', #25002 ) ;
#20325 = ORIENTED_EDGE ( 'NONE', *, *, #20106, .F. ) ;
#20326 = LINE ( 'NONE', #12352, #5029 ) ;
#20327 = CARTESIAN_POINT ( 'NONE',  ( 40.77203464402485622, 0.8961591335780867418, 71.43714994484035685 ) ) ;
#20328 = CARTESIAN_POINT ( 'NONE',  ( 37.25260217561390874, -23.61368208888610098, 71.78268878715390144 ) ) ;
#20329 = ORIENTED_EDGE ( 'NONE', *, *, #22859, .F. ) ;
#20330 = ORIENTED_EDGE ( 'NONE', *, *, #24621, .T. ) ;
#20331 = CARTESIAN_POINT ( 'NONE',  ( 33.81606138205700063, 16.19123852234699967, 69.30501292736995822 ) ) ;
#20332 = CARTESIAN_POINT ( 'NONE',  ( 36.80608444377001121, -1.313682088886099386, 70.35351908239860563 ) ) ;
#20333 = CARTESIAN_POINT ( 'NONE',  ( 39.98359781491296161, -29.20384086642191335, 70.89533451361944572 ) ) ;
#20334 = CIRCLE ( 'NONE', #19903, 1.750000000000000222 ) ;
#20335 = FACE_OUTER_BOUND ( 'NONE', #21517, .T. ) ;
#20336 = VECTOR ( 'NONE', #13268, 1000.000000000000000 ) ;
#20337 = CARTESIAN_POINT ( 'NONE',  ( 39.02088643472237095, -10.91368208888610170, 69.02690120949094421 ) ) ;
#20338 = ADVANCED_FACE ( 'NONE', ( #9080 ), #25126, .T. ) ;
#20339 = FACE_OUTER_BOUND ( 'NONE', #1571, .T. ) ;
#20340 = FACE_OUTER_BOUND ( 'NONE', #17335, .T. ) ;
#20341 = FACE_OUTER_BOUND ( 'NONE', #18798, .T. ) ;
#20342 = CARTESIAN_POINT ( 'NONE',  ( 39.66066260159681889, -29.10876147764981781, 69.85357445396793707 ) ) ;
#20343 = CARTESIAN_POINT ( 'NONE',  ( 37.80618814713140097, -1.913682088886106136, 73.13360434286904876 ) ) ;
#20344 = DIRECTION ( 'NONE',  ( -1.000000000000000000, 0.000000000000000000, 0.000000000000000000 ) ) ;
#20345 = CARTESIAN_POINT ( 'NONE',  ( 29.71606138205695657, -23.19619402982949907, 47.16846523730000484 ) ) ;
#20346 = ORIENTED_EDGE ( 'NONE', *, *, #7148, .F. ) ;
#20347 = DIRECTION ( 'NONE',  ( 4.341746501209495972E-16, -0.4341746501209495790, -0.9008287146801833289 ) ) ;
#20348 = MECHANICAL_DESIGN_GEOMETRIC_PRESENTATION_REPRESENTATION (  '', ( #8422 ), #21988 ) ;
#20349 = DIRECTION ( 'NONE',  ( -1.000000000000000000, 0.000000000000000000, 0.000000000000000000 ) ) ;
#20350 = ORIENTED_EDGE ( 'NONE', *, *, #25128, .F. ) ;
#20351 = ORIENTED_EDGE ( 'NONE', *, *, #2924, .F. ) ;
#20352 = CARTESIAN_POINT ( 'NONE',  ( 38.37017380507018771, -17.60384086642191193, 69.04448340153878405 ) ) ;
#20353 = CARTESIAN_POINT ( 'NONE',  ( 39.73277004305198545, 1.786317911113892043, 73.23812341099230139 ) ) ;
#20354 = FACE_OUTER_BOUND ( 'NONE', #9617, .T. ) ;
#20355 = DIRECTION ( 'NONE',  ( 1.734723475976804876E-16, -1.163336342344335610E-15, 1.000000000000000000 ) ) ;
#20356 = VERTEX_POINT ( 'NONE', #13319 ) ;
#20357 = LINE ( 'NONE', #14306, #3921 ) ;
#20358 = FACE_OUTER_BOUND ( 'NONE', #2095, .T. ) ;
#20359 = CARTESIAN_POINT ( 'NONE',  ( 40.52078840805428683, -24.61368208888610809, 70.60699637195608602 ) ) ;
#20360 = VECTOR ( 'NONE', #12670, 1000.000000000000000 ) ;
#20361 = EDGE_CURVE ( 'NONE', #22752, #20175, #3511, .T. ) ;
#20362 = LINE ( 'NONE', #12144, #16456 ) ;
#20364 = EDGE_CURVE ( 'NONE', #7242, #6145, #11072, .T. ) ;
#20363 = CARTESIAN_POINT ( 'NONE',  ( 38.31606138205700063, 12.69123852234700678, 71.30501292736997243 ) ) ;
#20365 = CARTESIAN_POINT ( 'NONE',  ( 39.75915168707250302, -8.713682088886097077, 70.26145752964252722 ) ) ;
#20366 = LINE ( 'NONE', #10456, #3082 ) ;
#20367 = CARTESIAN_POINT ( 'NONE',  ( 36.68196826583682935, -23.61368208888610454, 71.96809898377887293 ) ) ;
#20368 = CARTESIAN_POINT ( 'NONE',  ( 30.81606138205696510, -0.7562224151693580643, -1.633662118351544734 ) ) ;
#20369 = CARTESIAN_POINT ( 'NONE',  ( 41.31606138205700063, 1.207247317117632335, 63.73818242441765847 ) ) ;
#20370 = CARTESIAN_POINT ( 'NONE',  ( 37.60469502381300799, -22.40384086642191264, 72.26730301774234988 ) ) ;
#20371 = CARTESIAN_POINT ( 'NONE',  ( 39.98359781491296161, -10.41368208888610347, 71.86517103874048473 ) ) ;
#20372 = CARTESIAN_POINT ( 'NONE',  ( 33.80700705136447937, 3.227014435054107455, 6.369498925975481285 ) ) ;
#20373 = EDGE_CURVE ( 'NONE', #22901, #20176, #2412, .T. ) ;
#20374 = VERTEX_POINT ( 'NONE', #13065 ) ;
#20375 = VECTOR ( 'NONE', #16738, 1000.000000000000000 ) ;
#20376 = CARTESIAN_POINT ( 'NONE',  ( 36.64852494920107517, -12.20384086642190979, 71.86517103874048473 ) ) ;
#20377 = LINE ( 'NONE', #2584, #9773 ) ;
#20378 = CARTESIAN_POINT ( 'NONE',  ( 39.75915168707250302, -8.713682088886097077, 70.26145752964252722 ) ) ;
#20379 = ORIENTED_EDGE ( 'NONE', *, *, #881, .T. ) ;
#20380 = CARTESIAN_POINT ( 'NONE',  ( 36.07789103942398867, -13.41368208888610525, 70.70992431699450265 ) ) ;
#20381 = ORIENTED_EDGE ( 'NONE', *, *, #2372, .F. ) ;
#20382 = DIRECTION ( 'NONE',  ( -1.000000000000000000, -1.734723475976804876E-16, 1.734723475976814737E-16 ) ) ;
#20383 = CARTESIAN_POINT ( 'NONE',  ( 42.82259792697934841, 3.224889410007908630, 6.370942052746025652 ) ) ;
#20384 = CARTESIAN_POINT ( 'NONE',  ( 39.41296390513587511, -9.203840866421909794, 71.08074471024443142 ) ) ;
#20385 = DIRECTION ( 'NONE',  ( 0.000000000000000000, -1.000000000000000000, 0.000000000000000000 ) ) ;
#20386 = ORIENTED_EDGE ( 'NONE', *, *, #3719, .F. ) ;
#20387 = DIRECTION ( 'NONE',  ( 0.000000000000000000, -2.999999999999999839E-15, -1.000000000000000000 ) ) ;
#20388 = PLANE ( 'NONE',  #5069 ) ;
#20389 = CARTESIAN_POINT ( 'NONE',  ( 36.07789103942399578, -24.20384086642191690, 72.05058123536544201 ) ) ;
#20390 = CARTESIAN_POINT ( 'NONE',  ( 43.81606138205700063, 44.92314894770293421, 79.37823623207320622 ) ) ;
#20391 = CARTESIAN_POINT ( 'NONE',  ( 38.26194895904383486, -25.01368208888610312, 69.64448340153876416 ) ) ;
#20392 = CARTESIAN_POINT ( 'NONE',  ( 36.31606138205700063, -10.93995761290683255, 80.99653337025984001 ) ) ;
#20393 = DIRECTION ( 'NONE',  ( -1.000000000000000000, -1.000000000000000078E-15, 0.000000000000000000 ) ) ;
#20394 = ORIENTED_EDGE ( 'NONE', *, *, #17056, .T. ) ;
#20395 = DIRECTION ( 'NONE',  ( 0.000000000000000000, 1.000000000000000000, 0.000000000000000000 ) ) ;
#20396 = CARTESIAN_POINT ( 'NONE',  ( 32.56606138205700773, 43.04446929126255128, 81.37823623207322044 ) ) ;
#20397 = CARTESIAN_POINT ( 'NONE',  ( 37.69796330110505522, -16.50384086642191406, 73.09843995877329803 ) ) ;
#20398 = DIRECTION ( 'NONE',  ( 1.000000000000000000, 0.000000000000000000, 0.000000000000000000 ) ) ;
#20399 = CARTESIAN_POINT ( 'NONE',  ( 31.01606138205699992, 46.92314894770294131, 81.17823623207318917 ) ) ;
#20400 = CARTESIAN_POINT ( 'NONE',  ( 32.81606138205700773, 46.72314894770294558, 81.37823623207320622 ) ) ;
#20401 = EDGE_CURVE ( 'NONE', #24942, #17659, #2077, .T. ) ;
#20402 = LINE ( 'NONE', #12441, #17706 ) ;
#20403 = CARTESIAN_POINT ( 'NONE',  ( 36.87297107704149823, -27.90384086642190908, 70.26145752964251301 ) ) ;
#20404 = DIRECTION ( 'NONE',  ( 0.1803747433772529551, -0.9835979625596985576, 0.000000000000000000 ) ) ;
#20405 = ORIENTED_EDGE ( 'NONE', *, *, #1219, .F. ) ;
#20406 = CARTESIAN_POINT ( 'NONE',  ( 36.68196826583682935, -23.61368208888610454, 71.96809898377887293 ) ) ;
#20407 = VERTEX_POINT ( 'NONE', #8145 ) ;
#20408 = ORIENTED_EDGE ( 'NONE', *, *, #2374, .T. ) ;
#20409 = FACE_OUTER_BOUND ( 'NONE', #11239, .T. ) ;
#20410 = CARTESIAN_POINT ( 'NONE',  ( 33.31606138205700773, -5.204193249396356968, 72.80501292736992980 ) ) ;
#20411 = CARTESIAN_POINT ( 'NONE',  ( 39.02742774030101458, -29.40384086642191264, 70.49320253461758057 ) ) ;
#20412 = CARTESIAN_POINT ( 'NONE',  ( 39.31564783533280405, -0.3136820888861025503, 72.03616607671141026 ) ) ;
#20413 = ORIENTED_EDGE ( 'NONE', *, *, #19057, .F. ) ;
#20414 = ORIENTED_EDGE ( 'NONE', *, *, #2321, .T. ) ;
#20415 = FACE_OUTER_BOUND ( 'NONE', #10432, .T. ) ;
#20416 = LINE ( 'NONE', #6767, #24343 ) ;
#20417 = ORIENTED_EDGE ( 'NONE', *, *, #6176, .T. ) ;
#20418 = SURFACE_SIDE_STYLE ('',( #4961 ) ) ;
#20419 = CARTESIAN_POINT ( 'NONE',  ( 38.93415946300896024, -11.50384086642190340, 69.66206559358663242 ) ) ;
#20420 = EDGE_CURVE ( 'NONE', #13993, #6274, #3896, .T. ) ;
#20421 = SURFACE_STYLE_USAGE ( .BOTH. , #11850 ) ;
#20422 = EDGE_CURVE ( 'NONE', #11230, #19656, #9708, .T. ) ;
#20423 = DIRECTION ( 'NONE',  ( 8.758115402030106693E-47, -1.000000000000000000, 3.469446951953613400E-15 ) ) ;
#20424 = EDGE_CURVE ( 'NONE', #15753, #868, #16115, .T. ) ;
#20425 = EDGE_LOOP ( 'NONE', ( #6219, #11561, #13635, #11546, #20250, #21313 ) ) ;
#20426 = ADVANCED_FACE ( 'NONE', ( #6213 ), #7899, .T. ) ;
#20427 = ADVANCED_FACE ( 'NONE', ( #21924 ), #25387, .F. ) ;
#20428 = ORIENTED_EDGE ( 'NONE', *, *, #13490, .T. ) ;
#20429 = DIRECTION ( 'NONE',  ( -2.453269466693404537E-16, 0.7071067811865489050, -0.7071067811865460184 ) ) ;
#20430 = CARTESIAN_POINT ( 'NONE',  ( 39.98359781491296161, -8.413682088886105248, 71.86517103874048473 ) ) ;
#20431 = ORIENTED_EDGE ( 'NONE', *, *, #21284, .F. ) ;
#20432 = CARTESIAN_POINT ( 'NONE',  ( 40.56606138205700773, 2.740850673309605412, 6.112030963703427133 ) ) ;
#20433 = FACE_BOUND ( 'NONE', #21295, .T. ) ;
#20434 = DIRECTION ( 'NONE',  ( 0.000000000000000000, 2.999999999999999839E-15, 1.000000000000000000 ) ) ;
#20435 = EDGE_CURVE ( 'NONE', #723, #15261, #7769, .T. ) ;
#20436 = ADVANCED_FACE ( 'NONE', ( #15868 ), #12156, .T. ) ;
#20437 = CARTESIAN_POINT ( 'NONE',  ( 33.31606138205700773, -5.204193249396277032, 83.30501292736992980 ) ) ;
#20438 = CARTESIAN_POINT ( 'NONE',  ( 36.31606138205701484, -6.852252720116931428, 82.67173867183331026 ) ) ;
#20439 = CARTESIAN_POINT ( 'NONE',  ( 45.81606138205700063, 31.19260082947834078, 104.9690409559304101 ) ) ;
#20440 = ORIENTED_EDGE ( 'NONE', *, *, #7858, .T. ) ;
#20441 = EDGE_LOOP ( 'NONE', ( #22339, #3954, #15786, #21652 ) ) ;
#20442 = AXIS2_PLACEMENT_3D ( 'NONE', #20551, #20681, #22862 ) ;
#20443 = DIRECTION ( 'NONE',  ( 0.000000000000000000, -1.000000000000000000, 2.999999999999999839E-15 ) ) ;
#20444 = CARTESIAN_POINT ( 'NONE',  ( 40.26954217208372455, -0.9038408664219198529, 72.86986841596736042 ) ) ;
#20445 = AXIS2_PLACEMENT_3D ( 'NONE', #22324, #18839, #9071 ) ;
#20446 = CIRCLE ( 'NONE', #1103, 0.7500000000000031086 ) ;
#20447 = CARTESIAN_POINT ( 'NONE',  ( 39.31564783533280405, -24.31368208888610383, 72.03616607671136762 ) ) ;
#20448 = VERTEX_POINT ( 'NONE', #11771 ) ;
#20449 = EDGE_CURVE ( 'NONE', #20703, #24865, #9831, .T. ) ;
#20450 = ORIENTED_EDGE ( 'NONE', *, *, #12738, .F. ) ;
#20451 = DIRECTION ( 'NONE',  ( -1.734723475976805122E-16, -3.491481338843134933E-15, -1.000000000000000000 ) ) ;
#20452 = CARTESIAN_POINT ( 'NONE',  ( 37.69796330110504101, -3.113682088886098764, 69.66206559358663242 ) ) ;
#20453 = CARTESIAN_POINT ( 'NONE',  ( 40.14115730948191185, -29.10384086642190482, 71.43714994484028580 ) ) ;
#20454 = CARTESIAN_POINT ( 'NONE',  ( 33.81606138205700063, 2.191238522347013440, 73.80501292737000085 ) ) ;
#20455 = CARTESIAN_POINT ( 'NONE',  ( 39.02088643472237095, -6.913682088886101695, 69.02690120949094421 ) ) ;
#20456 = EDGE_CURVE ( 'NONE', #8796, #6972, #17675, .T. ) ;
#20457 = CARTESIAN_POINT ( 'NONE',  ( 32.81606138205700773, -27.52349462642295208, 56.67559192035834315 ) ) ;
#20458 = LINE ( 'NONE', #8878, #9989 ) ;
#20459 = CARTESIAN_POINT ( 'NONE',  ( 44.81606138205700063, 31.19260082947834078, 104.9690409559304101 ) ) ;
#20460 = VECTOR ( 'NONE', #17283, 1000.000000000000000 ) ;
#20461 = CARTESIAN_POINT ( 'NONE',  ( 39.59324923284151510, -28.74115096347518161, 70.20355626897213597 ) ) ;
#20462 = VECTOR ( 'NONE', #24206, 1000.000000000000114 ) ;
#20463 = CIRCLE ( 'NONE', #1946, 0.5000000000000004441 ) ;
#20464 = DIRECTION ( 'NONE',  ( -1.327674326049719602E-15, 0.4425581086832399147, -0.8967398287344627850 ) ) ;
#20465 = DIRECTION ( 'NONE',  ( -1.000000000000000000, 0.000000000000000000, 0.000000000000000000 ) ) ;
#20466 = ORIENTED_EDGE ( 'NONE', *, *, #16478, .F. ) ;
#20467 = CARTESIAN_POINT ( 'NONE',  ( 32.81606138205700773, -37.34243788671330577, 70.80615726751818784 ) ) ;
#20468 = DIRECTION ( 'NONE',  ( 0.000000000000000000, -0.8212051873014297732, -0.5706330172266793621 ) ) ;
#20469 = ORIENTED_EDGE ( 'NONE', *, *, #23357, .F. ) ;
#20470 = ORIENTED_EDGE ( 'NONE', *, *, #18614, .F. ) ;
#20471 = CARTESIAN_POINT ( 'NONE',  ( 40.33642880535521869, -15.30384086642191477, 69.98269868914866265 ) ) ;
#20472 = EDGE_CURVE ( 'NONE', #17699, #3791, #2329, .T. ) ;
#20473 = CARTESIAN_POINT ( 'NONE',  ( 39.82603832034400426, -20.31368208888610738, 72.40698646996133903 ) ) ;
#20474 = CARTESIAN_POINT ( 'NONE',  ( 42.81606138205700063, 22.19123852234699967, 69.30501292736994401 ) ) ;
#20475 = AXIS2_PLACEMENT_3D ( 'NONE', #19376, #23626, #5983 ) ;
#20476 = AXIS2_PLACEMENT_3D ( 'NONE', #5141, #20849, #23277 ) ;
#20477 = LINE ( 'NONE', #2939, #18840 ) ;
#20478 = DIRECTION ( 'NONE',  ( 0.000000000000000000, 1.000000000000000000, -2.775557561562891351E-15 ) ) ;
#20479 = ORIENTED_EDGE ( 'NONE', *, *, #14916, .T. ) ;
#20480 = CARTESIAN_POINT ( 'NONE',  ( 31.81606138205700418, 39.19123852234599070, 72.05501292736988717 ) ) ;
#20481 = DIRECTION ( 'NONE',  ( 0.000000000000000000, -1.000000000000000000, 2.999999999999999839E-15 ) ) ;
#20482 = CARTESIAN_POINT ( 'NONE',  ( 36.11133435605973574, -0.003840866421914862494, 70.60699637195612866 ) ) ;
#20483 = ORIENTED_EDGE ( 'NONE', *, *, #13906, .T. ) ;
#20484 = CYLINDRICAL_SURFACE ( 'NONE', #19757, 3.000000000000002665 ) ;
#20485 = LINE ( 'NONE', #4895, #16969 ) ;
#20486 = CARTESIAN_POINT ( 'NONE',  ( 36.80608444377001121, -3.313682088886100718, 70.35351908239860563 ) ) ;
#20487 = DIRECTION ( 'NONE',  ( 6.938893903907229364E-16, 0.8212051873014208914, 0.5706330172266919076 ) ) ;
#20488 = CARTESIAN_POINT ( 'NONE',  ( 37.33957961208646736, -21.81368208888610738, 72.81632618279321889 ) ) ;
#20489 = DIRECTION ( 'NONE',  ( -1.000000000000000000, -2.999999999999999839E-15, 0.000000000000000000 ) ) ;
#20490 = CIRCLE ( 'NONE', #17212, 1.250000000000000888 ) ;
#20491 = CYLINDRICAL_SURFACE ( 'NONE', #15779, 0.2000000000000057288 ) ;
#20492 = CARTESIAN_POINT ( 'NONE',  ( 39.41296390513587511, -21.20384086642190979, 71.08074471024441721 ) ) ;
#20493 = CARTESIAN_POINT ( 'NONE',  ( 39.98359781491296161, -6.413682088886103472, 71.86517103874048473 ) ) ;
#20494 = VECTOR ( 'NONE', #21865, 1000.000000000000114 ) ;
#20495 = ORIENTED_EDGE ( 'NONE', *, *, #25058, .F. ) ;
#20496 = DIRECTION ( 'NONE',  ( 0.000000000000000000, -1.000000000000000000, 2.999999999999999839E-15 ) ) ;
#20497 = EDGE_LOOP ( 'NONE', ( #4295, #11068, #15274, #11038, #2709, #13639 ) ) ;
#20498 = EDGE_CURVE ( 'NONE', #9852, #20804, #4157, .T. ) ;
#20499 = CARTESIAN_POINT ( 'NONE',  ( 39.38009889167648936, -3.403840866421908196, 70.00779233799264034 ) ) ;
#20500 = LINE ( 'NONE', #14825, #15508 ) ;
#20501 = ADVANCED_FACE ( 'NONE', ( #5963 ), #14205, .T. ) ;
#20502 = EDGE_CURVE ( 'NONE', #15148, #20448, #265, .T. ) ;
#20503 = CARTESIAN_POINT ( 'NONE',  ( 38.37017380507020192, -6.013682088886109334, 73.11602215082118050 ) ) ;
#20504 = ORIENTED_EDGE ( 'NONE', *, *, #10564, .T. ) ;
#20505 = CARTESIAN_POINT ( 'NONE',  ( 40.52078840805428683, -10.61368208888610631, 70.60699637195608602 ) ) ;
#20506 = EDGE_LOOP ( 'NONE', ( #1831, #9464, #20065, #3576 ) ) ;
#20507 = DIRECTION ( 'NONE',  ( 0.000000000000000000, -3.965082230804126670E-15, -1.000000000000000000 ) ) ;
#20508 = DIRECTION ( 'NONE',  ( 0.000000000000000000, 3.469446951953613400E-15, 1.000000000000000000 ) ) ;
#20509 = CARTESIAN_POINT ( 'NONE',  ( 37.31647492878124694, -14.30384086642191122, 72.03616607671141026 ) ) ;
#20510 = LINE ( 'NONE', #10857, #10613 ) ;
#20511 = ORIENTED_EDGE ( 'NONE', *, *, #22406, .F. ) ;
#20512 = FACE_OUTER_BOUND ( 'NONE', #9462, .T. ) ;
#20513 = CARTESIAN_POINT ( 'NONE',  ( 32.56606138205700773, 47.04446929126254417, 81.37823623207319201 ) ) ;
#20514 = CARTESIAN_POINT ( 'NONE',  ( 36.29569395875881099, -14.30384086642192010, 72.77780686321128201 ) ) ;
#20515 = DIRECTION ( 'NONE',  ( 1.000000000000000000, 0.000000000000000000, 0.000000000000000000 ) ) ;
#20516 = AXIS2_PLACEMENT_3D ( 'NONE', #23497, #2108, #12184 ) ;
#20517 = CARTESIAN_POINT ( 'NONE',  ( 36.49096545463212493, -19.51368208888610312, 71.43714994484034264 ) ) ;
#20518 = CARTESIAN_POINT ( 'NONE',  ( 15.14989484155900001, 36.04731275961434989, 83.30501292736985874 ) ) ;
#20519 = EDGE_CURVE ( 'NONE', #12687, #13086, #21668, .T. ) ;
#20520 = LINE ( 'NONE', #18586, #19607 ) ;
#20521 = VERTEX_POINT ( 'NONE', #11894 ) ;
#20522 = CARTESIAN_POINT ( 'NONE',  ( 44.06606138205700063, 43.35512946304240245, 83.12823623207320622 ) ) ;
#20523 = DIRECTION ( 'NONE',  ( 0.000000000000000000, -0.5706330172266919076, 0.8212051873014208914 ) ) ;
#20524 = CARTESIAN_POINT ( 'NONE',  ( 36.49096545463212493, -16.10384086642191548, 71.32335560751961623 ) ) ;
#20525 = CARTESIAN_POINT ( 'NONE',  ( 31.81606138205700418, 35.95440708241085304, 62.30501292736990138 ) ) ;
#20526 = AXIS2_PLACEMENT_3D ( 'NONE', #6677, #14792, #24308 ) ;
#20527 = CARTESIAN_POINT ( 'NONE',  ( 29.81606138205697576, -4.349482454670887677, -5.142398479549302515 ) ) ;
#20528 = CIRCLE ( 'NONE', #24622, 1.000000000000000888 ) ;
#20529 = DIRECTION ( 'NONE',  ( 0.000000000000000000, -0.8212051873014210024, -0.5706330172266920187 ) ) ;
#20530 = CARTESIAN_POINT ( 'NONE',  ( 39.29254315202757653, -24.80384086642191477, 72.81632618279320468 ) ) ;
#20531 = CARTESIAN_POINT ( 'NONE',  ( 36.57819145821473228, -6.157615413744179200, 82.75497663158847672 ) ) ;
#20532 = ORIENTED_EDGE ( 'NONE', *, *, #21227, .F. ) ;
#20533 = AXIS2_PLACEMENT_3D ( 'NONE', #19736, #17818, #149 ) ;
#20534 = CARTESIAN_POINT ( 'NONE',  ( 38.82593461698262871, -24.91368208888610170, 69.62690120949091011 ) ) ;
#20535 = ORIENTED_EDGE ( 'NONE', *, *, #11009, .T. ) ;
#20536 = ORIENTED_EDGE ( 'NONE', *, *, #10660, .T. ) ;
#20537 = DIRECTION ( 'NONE',  ( 0.000000000000000000, 2.999999999999999839E-15, 1.000000000000000000 ) ) ;
#20538 = PLANE ( 'NONE',  #12084 ) ;
#20539 = CARTESIAN_POINT ( 'NONE',  ( 37.38336156205273397, -27.90384086642191264, 70.63227792289245599 ) ) ;
#20540 = VECTOR ( 'NONE', #3472, 1000.000000000000000 ) ;
#20541 = CARTESIAN_POINT ( 'NONE',  ( 39.02742774030102879, -0.2136820888860996304, 72.26730301774236409 ) ) ;
#20542 = ORIENTED_EDGE ( 'NONE', *, *, #17368, .T. ) ;
#20543 = ORIENTED_EDGE ( 'NONE', *, *, #13692, .T. ) ;
#20544 = DIRECTION ( 'NONE',  ( 0.000000000000000000, 0.000000000000000000, 1.000000000000000000 ) ) ;
#20545 = CARTESIAN_POINT ( 'NONE',  ( 33.31606138205700773, 3.195231713396695650, 64.80689721350518084 ) ) ;
#20546 = ORIENTED_EDGE ( 'NONE', *, *, #12093, .F. ) ;
#20547 = LINE ( 'NONE', #24266, #23495 ) ;
#20548 = CARTESIAN_POINT ( 'NONE',  ( 37.33957961208645315, -1.803840866421907441, 69.94417936956673998 ) ) ;
#20549 = VECTOR ( 'NONE', #13978, 1000.000000000000000 ) ;
#20550 = EDGE_CURVE ( 'NONE', #19348, #22473, #9860, .T. ) ;
#20551 = CARTESIAN_POINT ( 'NONE',  ( 38.31606138205700063, -6.959910619544160681, 20.07251914782758107 ) ) ;
#20552 = ORIENTED_EDGE ( 'NONE', *, *, #2778, .F. ) ;
#20553 = EDGE_LOOP ( 'NONE', ( #4073, #7567, #10101, #14669 ) ) ;
#20554 = ORIENTED_EDGE ( 'NONE', *, *, #1906, .F. ) ;
#20555 = AXIS2_PLACEMENT_3D ( 'NONE', #116, #17891, #13532 ) ;
#20556 = FACE_OUTER_BOUND ( 'NONE', #22679, .T. ) ;
#20557 = CARTESIAN_POINT ( 'NONE',  ( 39.82603832034401847, 1.686317911113892176, 72.40698646996135324 ) ) ;
#20558 = DIRECTION ( 'NONE',  ( -2.120312145707929538E-16, 0.8213699656732942334, -0.5703958094953462954 ) ) ;
#20559 = LINE ( 'NONE', #8725, #18238 ) ;
#20560 = VECTOR ( 'NONE', #11524, 1000.000000000000000 ) ;
#20561 = AXIS2_PLACEMENT_3D ( 'NONE', #7523, #5459, #19489 ) ;
#20562 = DIRECTION ( 'NONE',  ( 1.000000000000000000, 0.000000000000000000, 0.000000000000000000 ) ) ;
#20563 = AXIS2_PLACEMENT_3D ( 'NONE', #13788, #25356, #21388 ) ;
#20564 = CARTESIAN_POINT ( 'NONE',  ( 43.31606138205700773, -19.13113579875041381, 24.60350147050422720 ) ) ;
#20565 = LINE ( 'NONE', #10659, #2790 ) ;
#20566 = EDGE_CURVE ( 'NONE', #8460, #5709, #23717, .T. ) ;
#20567 = EDGE_CURVE ( 'NONE', #6977, #5267, #17947, .T. ) ;
#20568 = FACE_OUTER_BOUND ( 'NONE', #21331, .T. ) ;
#20569 = ORIENTED_EDGE ( 'NONE', *, *, #2098, .T. ) ;
#20570 = ORIENTED_EDGE ( 'NONE', *, *, #15871, .F. ) ;
#20571 = CARTESIAN_POINT ( 'NONE',  ( 41.31606138205687273, 42.19123852234596939, 65.30501292736988717 ) ) ;
#20572 = CARTESIAN_POINT ( 'NONE',  ( 38.31606138205700063, 15.19123852234700500, 71.30501292736995822 ) ) ;
#20573 = ADVANCED_FACE ( 'NONE', ( #2453 ), #24212, .F. ) ;
#20574 = CARTESIAN_POINT ( 'NONE',  ( 39.41296390513587511, -20.41368208888610170, 71.67976084211551324 ) ) ;
#20575 = ORIENTED_EDGE ( 'NONE', *, *, #20753, .F. ) ;
#20576 = ORIENTED_EDGE ( 'NONE', *, *, #5307, .F. ) ;
#20577 = DIRECTION ( 'NONE',  ( -8.758115402030106693E-47, 1.000000000000000000, -3.469446951953613400E-15 ) ) ;
#20578 = CARTESIAN_POINT ( 'NONE',  ( 37.80618814713140097, -3.913682088886108801, 73.13360434286904876 ) ) ;
#20579 = CARTESIAN_POINT ( 'NONE',  ( 36.49096545463212493, -28.10384086642190127, 71.32335560751960202 ) ) ;
#20580 = CARTESIAN_POINT ( 'NONE',  ( 36.31606138205700063, -11.22674583108233115, 81.40610939240433197 ) ) ;
#20581 = EDGE_CURVE ( 'NONE', #7686, #18144, #16752, .T. ) ;
#20582 = CARTESIAN_POINT ( 'NONE',  ( 39.73277004305198545, -6.213682088886108623, 73.23812341099225875 ) ) ;
#20583 = VECTOR ( 'NONE', #11584, 1000.000000000000000 ) ;
#20584 = DIRECTION ( 'NONE',  ( 1.000000000000000000, 0.000000000000000000, 0.000000000000000000 ) ) ;
#20585 = DIRECTION ( 'NONE',  ( 0.000000000000000000, 0.6568589528324746407, -0.7540134720837716742 ) ) ;
#20586 = DIRECTION ( 'NONE',  ( -2.792262043613788535E-15, 0.8967398287344627850, 0.4425581086832399147 ) ) ;
#20587 = ADVANCED_BREP_SHAPE_REPRESENTATION ( '', ( #8266, #2000 ), #2615 ) ;
#20588 = CARTESIAN_POINT ( 'NONE',  ( 32.56606138205700773, 40.92314894770289158, 83.08534301325974525 ) ) ;
#20589 = CARTESIAN_POINT ( 'NONE',  ( 39.54057891361352972, -5.597492753917878261, 82.79251829992152523 ) ) ;
#20590 = CARTESIAN_POINT ( 'NONE',  ( 42.96606138205698500, -7.467730535347522292, -2.778285769174305919 ) ) ;
#20591 = DIRECTION ( 'NONE',  ( 0.000000000000000000, 0.6568589528324746407, -0.7540134720837716742 ) ) ;
#20592 = EDGE_CURVE ( 'NONE', #5274, #22820, #9443, .T. ) ;
#20593 = VERTEX_POINT ( 'NONE', #14569 ) ;
#20594 = EDGE_CURVE ( 'NONE', #19306, #21783, #22295, .T. ) ;
#20595 = VECTOR ( 'NONE', #2380, 1000.000000000000000 ) ;
#20596 = DIRECTION ( 'NONE',  ( 0.000000000000000000, 1.000000000000000000, -2.999999999999999839E-15 ) ) ;
#20597 = DIRECTION ( 'NONE',  ( 0.000000000000000000, -0.6568589528324746407, 0.7540134720837716742 ) ) ;
#20598 = ORIENTED_EDGE ( 'NONE', *, *, #13521, .T. ) ;
#20599 = EDGE_CURVE ( 'NONE', #5938, #21676, #12783, .T. ) ;
#20600 = VERTEX_POINT ( 'NONE', #24589 ) ;
#20601 = UNCERTAINTY_MEASURE_WITH_UNIT (LENGTH_MEASURE( 1.000000000000000082E-05 ), #21242, 'distance_accuracy_value', 'NONE');
#20602 = AXIS2_PLACEMENT_3D ( 'NONE', #10405, #4482, #23790 ) ;
#20603 = CARTESIAN_POINT ( 'NONE',  ( 36.29569395875881099, -14.30384086642192010, 72.77780686321128201 ) ) ;
#20604 = EDGE_CURVE ( 'NONE', #17894, #15622, #4658, .T. ) ;
#20605 = EDGE_CURVE ( 'NONE', #7382, #23154, #1029, .T. ) ;
#20606 = CARTESIAN_POINT ( 'NONE',  ( 39.82603832034400426, -24.31368208888611093, 72.40698646996131060 ) ) ;
#20607 = PLANE ( 'NONE',  #14834 ) ;
#20608 = CARTESIAN_POINT ( 'NONE',  ( 40.31606138205700773, -29.30876147765400219, 74.30501292737010033 ) ) ;
#20609 = SURFACE_STYLE_USAGE ( .BOTH. , #24834 ) ;
#20610 = ORIENTED_EDGE ( 'NONE', *, *, #8626, .F. ) ;
#20611 = DIRECTION ( 'NONE',  ( -1.000000000000000000, 0.000000000000000000, 0.000000000000000000 ) ) ;
#20612 = PLANE ( 'NONE',  #560 ) ;
#20613 = ADVANCED_FACE ( 'NONE', ( #22047 ), #4408, .F. ) ;
#20614 = CARTESIAN_POINT ( 'NONE',  ( 36.11133435605973574, -27.61368208888610809, 72.15350918040381600 ) ) ;
#20615 = ORIENTED_EDGE ( 'NONE', *, *, #21451, .F. ) ;
#20616 = CYLINDRICAL_SURFACE ( 'NONE', #8204, 0.9999999999999937828 ) ;
#20617 = CARTESIAN_POINT ( 'NONE',  ( 47.84183937708599643, -34.55876147765400219, 70.30501292737000085 ) ) ;
#20618 = CARTESIAN_POINT ( 'NONE',  ( 37.80618814713140097, -3.913682088886108801, 73.13360434286904876 ) ) ;
#20619 = CARTESIAN_POINT ( 'NONE',  ( 35.31606138205700773, 1.207247317117632335, 63.73818242441765847 ) ) ;
#20620 = CARTESIAN_POINT ( 'NONE',  ( 36.64852494920107517, -17.41368208888610525, 70.89533451361947414 ) ) ;
#20621 = DIRECTION ( 'NONE',  ( 0.000000000000000000, -2.999999999999999839E-15, -1.000000000000000000 ) ) ;
#20622 = EDGE_CURVE ( 'NONE', #3766, #19561, #7742, .T. ) ;
#20623 = CARTESIAN_POINT ( 'NONE',  ( 29.81606138205696155, -0.2703287878658162113, 1.505452687840413972 ) ) ;
#20624 = CARTESIAN_POINT ( 'NONE',  ( 39.51027997493896748, -19.10384086642191193, 71.43714994484032843 ) ) ;
#20625 = CARTESIAN_POINT ( 'NONE',  ( 37.69796330110504101, -5.113682088886101873, 69.66206559358663242 ) ) ;
#20626 = CARTESIAN_POINT ( 'NONE',  ( 33.31606138205700773, -10.93995761290683255, 80.99653337025984001 ) ) ;
#20627 = EDGE_LOOP ( 'NONE', ( #5463, #11103, #2284, #11422, #14333, #289, #12611, #22846, #24030, #21899 ) ) ;
#20628 = CARTESIAN_POINT ( 'NONE',  ( 36.68196826583682935, -8.003840866421912281, 70.79240656858108593 ) ) ;
#20629 = EDGE_CURVE ( 'NONE', #5882, #13733, #13550, .T. ) ;
#20630 = DIRECTION ( 'NONE',  ( -2.792262043613788535E-15, 0.8967398287344627850, 0.4425581086832399147 ) ) ;
#20631 = CARTESIAN_POINT ( 'NONE',  ( 39.98359781491296161, -8.413682088886105248, 71.86517103874048473 ) ) ;
#20632 = ORIENTED_EDGE ( 'NONE', *, *, #2521, .T. ) ;
#20633 = CARTESIAN_POINT ( 'NONE',  ( 39.64521430340304420, -10.81368208888610027, 69.45876917294177133 ) ) ;
#20634 = ORIENTED_EDGE ( 'NONE', *, *, #2925, .T. ) ;
#20635 = DIRECTION ( 'NONE',  ( -2.727049986597864201E-15, 0.7516416929448760387, 0.6595716529892418079 ) ) ;
#20636 = CARTESIAN_POINT ( 'NONE',  ( 38.63098279924290068, -10.70384086642191335, 72.53360434286905445 ) ) ;
#20637 = VERTEX_POINT ( 'NONE', #2580 ) ;
#20638 = DIRECTION ( 'NONE',  ( 0.000000000000000000, -1.000000000000000000, 2.999999999999999839E-15 ) ) ;
#20639 = DIRECTION ( 'NONE',  ( 0.000000000000000000, 0.000000000000000000, 1.000000000000000000 ) ) ;
#20640 = MECHANICAL_DESIGN_GEOMETRIC_PRESENTATION_REPRESENTATION (  '', ( #12018 ), #7472 ) ;
#20641 = CARTESIAN_POINT ( 'NONE',  ( 39.64521430340305841, -16.80384086642191832, 73.30173637941818754 ) ) ;
#20642 = CARTESIAN_POINT ( 'NONE',  ( 36.31606138205700063, -20.35033391287788973, 75.47555661361914758 ) ) ;
#20643 =( NAMED_UNIT ( * ) SI_UNIT ( $, .STERADIAN. ) SOLID_ANGLE_UNIT ( ) );
#20644 = CARTESIAN_POINT ( 'NONE',  ( 37.80618814713140097, -17.91368208888609814, 73.13360434286903455 ) ) ;
#20645 = DIRECTION ( 'NONE',  ( -9.925461516413211857E-16, 0.8967398287344598984, 0.4425581086832454658 ) ) ;
#20646 = CARTESIAN_POINT ( 'NONE',  ( 43.06606138205700063, 43.19123852234595518, 61.30501292736988006 ) ) ;
#20647 = EDGE_CURVE ( 'NONE', #19154, #23854, #4900, .T. ) ;
#20648 = ORIENTED_EDGE ( 'NONE', *, *, #20754, .F. ) ;
#20649 = EDGE_CURVE ( 'NONE', #2026, #25158, #11926, .T. ) ;
#20650 = CARTESIAN_POINT ( 'NONE',  ( 36.31606138205700063, 39.69123852234597649, 69.30501292736988717 ) ) ;
#20651 = DIRECTION ( 'NONE',  ( -0.000000000000000000, 0.5735764363510441610, -0.8191520442889931308 ) ) ;
#20652 = PRODUCT_DEFINITION ( 'UNKNOWN', '', #16631, #24944 ) ;
#20653 = CIRCLE ( 'NONE', #23446, 3.000000000000000000 ) ;
#20654 = CARTESIAN_POINT ( 'NONE',  ( 38.37017380507018771, -15.60384086642190837, 69.64448340153877837 ) ) ;
#20655 = CARTESIAN_POINT ( 'NONE',  ( 0.000000000000000000, 0.000000000000000000, 0.000000000000000000 ) ) ;
#20656 = AXIS2_PLACEMENT_3D ( 'NONE', #22437, #5401, #25206 ) ;
#20657 = CARTESIAN_POINT ( 'NONE',  ( 45.81606138205697221, -6.210967385200538260, -3.065230171572501661 ) ) ;
#20658 = CARTESIAN_POINT ( 'NONE',  ( 40.14115730948191185, -24.51368208888609601, 71.32335560751958781 ) ) ;
#20659 = APPLICATION_CONTEXT ( 'automotive_design' ) ;
#20660 = CARTESIAN_POINT ( 'NONE',  ( 32.31606138205700063, -20.88462213365835041, 44.49284693532412405 ) ) ;
#20661 = AXIS2_PLACEMENT_3D ( 'NONE', #14192, #10452, #8516 ) ;
#20662 = CARTESIAN_POINT ( 'NONE',  ( 38.37017380507018771, -23.60384086642190837, 69.64448340153877837 ) ) ;
#20663 = CARTESIAN_POINT ( 'NONE',  ( 36.36697178183959522, -6.614097045028025867, 82.70277949957684882 ) ) ;
#20664 = EDGE_CURVE ( 'NONE', #11095, #828, #772, .T. ) ;
#20665 = CARTESIAN_POINT ( 'NONE',  ( 37.80618814713140097, -25.91368208888610880, 73.13360434286902034 ) ) ;
#20666 = EDGE_LOOP ( 'NONE', ( #5547, #15646 ) ) ;
#20667 = EDGE_LOOP ( 'NONE', ( #19767, #1829, #12032, #4683 ) ) ;
#20668 = CARTESIAN_POINT ( 'NONE',  ( 43.81606138205700063, -2.373793412309109563, 19.60611914621674146 ) ) ;
#20669 = DIRECTION ( 'NONE',  ( -1.734723475976804876E-16, -3.469446951953610245E-15, -1.000000000000000000 ) ) ;
#20670 = CARTESIAN_POINT ( 'NONE',  ( 37.38336156205274818, -1.713682088886100852, 72.12822762946751709 ) ) ;
#20671 = CARTESIAN_POINT ( 'NONE',  ( 39.02742774030102879, 1.786317911113898704, 72.26730301774236409 ) ) ;
#20672 = ORIENTED_EDGE ( 'NONE', *, *, #8684, .T. ) ;
#20673 = ORIENTED_EDGE ( 'NONE', *, *, #12439, .T. ) ;
#20674 = CARTESIAN_POINT ( 'NONE',  ( 31.81606138205700418, 18.19123852234599070, 72.05501292736995822 ) ) ;
#20675 = LINE ( 'NONE', #1338, #22749 ) ;
#20676 = ORIENTED_EDGE ( 'NONE', *, *, #2611, .F. ) ;
#20677 = CARTESIAN_POINT ( 'NONE',  ( 37.33957961208645315, -5.803840866421907663, 69.94417936956673998 ) ) ;
#20678 = VECTOR ( 'NONE', #8748, 1000.000000000000000 ) ;
#20679 = DIRECTION ( 'NONE',  ( 0.000000000000000000, -0.6568589528324746407, 0.7540134720837716742 ) ) ;
#20680 = AXIS2_PLACEMENT_3D ( 'NONE', #12586, #14249, #22093 ) ;
#20681 = DIRECTION ( 'NONE',  ( -1.849283715844614702E-16, 0.8212051873014210024, 0.5706330172266920187 ) ) ;
#20682 = EDGE_LOOP ( 'NONE', ( #10648, #15840, #24635, #5004 ) ) ;
#20683 = ORIENTED_EDGE ( 'NONE', *, *, #25045, .F. ) ;
#20684 = EDGE_CURVE ( 'NONE', #24942, #12724, #2823, .T. ) ;
#20685 = ORIENTED_EDGE ( 'NONE', *, *, #12616, .T. ) ;
#20686 = ADVANCED_FACE ( 'NONE', ( #16245 ), #6463, .F. ) ;
#20687 = DIRECTION ( 'NONE',  ( 1.000000000000000000, 0.000000000000000000, 0.000000000000000000 ) ) ;
#20688 = CARTESIAN_POINT ( 'NONE',  ( 39.82603832034401847, -4.313682088886108268, 72.40698646996133903 ) ) ;
#20689 = AXIS2_PLACEMENT_3D ( 'NONE', #18032, #16080, #23929 ) ;
#20690 = AXIS2_PLACEMENT_3D ( 'NONE', #8360, #13896, #21752 ) ;
#20691 = DIRECTION ( 'NONE',  ( 1.000000000000000000, 2.999999999999999839E-15, 0.000000000000000000 ) ) ;
#20692 = CARTESIAN_POINT ( 'NONE',  ( 38.48938833801555148, 40.69123852234599781, 72.28987726642291989 ) ) ;
#20693 = CARTESIAN_POINT ( 'NONE',  ( 43.23147868389327897, 41.67000142393845152, 79.37823623207322044 ) ) ;
#20694 = VECTOR ( 'NONE', #7034, 1000.000000000000000 ) ;
#20695 = LINE ( 'NONE', #3291, #1808 ) ;
#20696 = VECTOR ( 'NONE', #23366, 1000.000000000000000 ) ;
#20697 = PLANE ( 'NONE',  #1608 ) ;
#20698 = CARTESIAN_POINT ( 'NONE',  ( 37.11263866765397523, -5.585986591960282688, 82.79779740004656219 ) ) ;
#20699 =( NAMED_UNIT ( * ) PLANE_ANGLE_UNIT ( ) SI_UNIT ( $, .RADIAN. ) );
#20700 = EDGE_CURVE ( 'NONE', #13391, #2408, #12655, .T. ) ;
#20701 = DIRECTION ( 'NONE',  ( 0.000000000000000000, 1.000000000000000000, 0.000000000000000000 ) ) ;
#20702 = ORIENTED_EDGE ( 'NONE', *, *, #14232, .T. ) ;
#20703 = VERTEX_POINT ( 'NONE', #18566 ) ;
#20704 = CARTESIAN_POINT ( 'NONE',  ( 32.81606138205700773, -3.566646240838321269, 18.16837712155798457 ) ) ;
#20705 = DIRECTION ( 'NONE',  ( -1.000000000000000000, 0.000000000000000000, 0.000000000000000000 ) ) ;
#20706 = CARTESIAN_POINT ( 'NONE',  ( 37.89291511884476904, -15.11368208888610098, 70.26206559358661252 ) ) ;
#20707 = ORIENTED_EDGE ( 'NONE', *, *, #16759, .T. ) ;
#20708 = AXIS2_PLACEMENT_3D ( 'NONE', #24277, #12467, #7026 ) ;
#20709 = ORIENTED_EDGE ( 'NONE', *, *, #4430, .T. ) ;
#20710 = DIRECTION ( 'NONE',  ( 2.602085213965210642E-15, -0.8967398287344635621, -0.4425581086832386379 ) ) ;
#20711 = CARTESIAN_POINT ( 'NONE',  ( 40.14115730948191185, -2.513682088886103116, 71.32335560751961623 ) ) ;
#20712 = CARTESIAN_POINT ( 'NONE',  ( 38.26194895904384907, -22.60384086642191548, 73.11602215082116629 ) ) ;
#20713 = LINE ( 'NONE', #16845, #5457 ) ;
#20714 = CARTESIAN_POINT ( 'NONE',  ( 40.77203464402485622, -8.513682088886104893, 71.32335560751961623 ) ) ;
#20715 = AXIS2_PLACEMENT_3D ( 'NONE', #20657, #2613, #10495 ) ;
#20716 = DIRECTION ( 'NONE',  ( -1.000000000000000000, 0.000000000000000000, 0.000000000000000000 ) ) ;
#20717 = ORIENTED_EDGE ( 'NONE', *, *, #24724, .F. ) ;
#20718 = CARTESIAN_POINT ( 'NONE',  ( 39.64148445914975127, -5.700736305954877459, 83.29367725972169012 ) ) ;
#20719 = VECTOR ( 'NONE', #10949, 1000.000000000000227 ) ;
#20720 = VERTEX_POINT ( 'NONE', #897 ) ;
#20721 = CARTESIAN_POINT ( 'NONE',  ( 44.81606138205700063, -34.55876147765403061, 66.30501292737011454 ) ) ;
#20722 = CARTESIAN_POINT ( 'NONE',  ( 43.31606138205697221, -5.022037326221694187, -5.474317061061731771 ) ) ;
#20723 = CARTESIAN_POINT ( 'NONE',  ( 40.30346352106939634, -6.862507256641427134, 82.66731276300377829 ) ) ;
#20724 = AXIS2_PLACEMENT_3D ( 'NONE', #23864, #23490, #4936 ) ;
#20725 = CARTESIAN_POINT ( 'NONE',  ( 33.31606138205700773, -33.60910547091194900, 60.61426200347987248 ) ) ;
#20726 = DIRECTION ( 'NONE',  ( 1.000000000000000000, 7.979170143241514824E-17, -1.148292460158762122E-16 ) ) ;
#20727 = ORIENTED_EDGE ( 'NONE', *, *, #16044, .T. ) ;
#20728 =( GEOMETRIC_REPRESENTATION_CONTEXT ( 3 ) GLOBAL_UNCERTAINTY_ASSIGNED_CONTEXT ( ( #4633 ) ) GLOBAL_UNIT_ASSIGNED_CONTEXT ( ( #1771, #25337, #23416 ) ) REPRESENTATION_CONTEXT ( 'NONE', 'WORKASPACE' ) );
#20729 = DIRECTION ( 'NONE',  ( -0.000000000000000000, 1.000000000000000000, -3.225463739888140187E-15 ) ) ;
#20730 = EDGE_CURVE ( 'NONE', #10306, #17769, #16001, .T. ) ;
#20731 = DIRECTION ( 'NONE',  ( 1.000000000000000000, 0.000000000000000000, 0.000000000000000000 ) ) ;
#20732 = EDGE_LOOP ( 'NONE', ( #14659, #18804, #4357, #21961 ) ) ;
#20733 = ORIENTED_EDGE ( 'NONE', *, *, #15389, .T. ) ;
#20734 = AXIS2_PLACEMENT_3D ( 'NONE', #7092, #23296, #7473 ) ;
#20735 = CARTESIAN_POINT ( 'NONE',  ( 38.37017380507018771, -15.60384086642191370, 69.04448340153878405 ) ) ;
#20736 = PRESENTATION_LAYER_ASSIGNMENT (  '', '', ( #4700 ) ) ;
#20737 = CARTESIAN_POINT ( 'NONE',  ( 36.49096545463212493, -19.51368208888610312, 71.43714994484034264 ) ) ;
#20738 = PLANE ( 'NONE',  #9922 ) ;
#20739 = DIRECTION ( 'NONE',  ( 1.327674326049719602E-15, -0.4425581086832399147, 0.8967398287344627850 ) ) ;
#20740 = EDGE_LOOP ( 'NONE', ( #14872, #12325, #4593, #12987 ) ) ;
#20741 = DIRECTION ( 'NONE',  ( -6.938893903907229955E-15, 1.000000000000000000, -2.999999999999999050E-15 ) ) ;
#20742 = CARTESIAN_POINT ( 'NONE',  ( 45.81606138205695800, -0.7562224151693129892, -1.633662118351544734 ) ) ;
#20743 = CARTESIAN_POINT ( 'NONE',  ( 35.86008812008917346, -0.1038408664219142574, 71.32335560751961623 ) ) ;
#20744 = EDGE_LOOP ( 'NONE', ( #23795, #22498, #10151, #15446 ) ) ;
#20745 = EDGE_CURVE ( 'NONE', #8842, #13774, #24970, .T. ) ;
#20746 = CARTESIAN_POINT ( 'NONE',  ( 45.81606138205695089, 1.361611432489176821, -2.592146606185703916 ) ) ;
#20747 = CARTESIAN_POINT ( 'NONE',  ( 37.25202387243752611, 0.7863179111138978161, 70.00779233799264034 ) ) ;
#20748 = DIRECTION ( 'NONE',  ( -1.000000000000000000, 0.000000000000000000, 0.000000000000000000 ) ) ;
#20749 = EDGE_CURVE ( 'NONE', #15791, #9810, #9424, .T. ) ;
#20750 = CARTESIAN_POINT ( 'NONE',  ( 37.25202387243752611, -23.21368208888610241, 70.00779233799262613 ) ) ;
#20751 = AXIS2_PLACEMENT_3D ( 'NONE', #23349, #21812, #17449 ) ;
#20752 = AXIS2_PLACEMENT_3D ( 'NONE', #3136, #15117, #24630 ) ;
#20753 = EDGE_CURVE ( 'NONE', #8442, #16850, #4106, .T. ) ;
#20754 = EDGE_CURVE ( 'NONE', #23347, #24520, #11355, .T. ) ;
#20755 = CARTESIAN_POINT ( 'NONE',  ( 40.31606138205700773, -20.56964486282017646, 75.94625445116911067 ) ) ;
#20756 = AXIS2_PLACEMENT_3D ( 'NONE', #541, #663, #16382 ) ;
#20757 = PLANE ( 'NONE',  #14157 ) ;
#20758 = CARTESIAN_POINT ( 'NONE',  ( 38.00113996487112189, -17.70384086642190979, 70.22690120949090442 ) ) ;
#20759 = CARTESIAN_POINT ( 'NONE',  ( 37.25202387243752611, -5.213682088886100630, 70.00779233799264034 ) ) ;
#20760 = DIRECTION ( 'NONE',  ( -1.000000000000000000, 0.000000000000000000, 0.000000000000000000 ) ) ;
#20761 = EDGE_CURVE ( 'NONE', #15185, #7399, #6146, .T. ) ;
#20762 = ORIENTED_EDGE ( 'NONE', *, *, #15213, .T. ) ;
#20763 = EDGE_CURVE ( 'NONE', #13486, #11800, #3480, .T. ) ;
#20764 = CARTESIAN_POINT ( 'NONE',  ( 38.82593461698265003, -4.703840866421914235, 73.13360434286904876 ) ) ;
#20765 = DIRECTION ( 'NONE',  ( 3.491481338843135327E-15, -1.000000000000000000, 2.999999999999999839E-15 ) ) ;
#20766 = COLOUR_RGB ( '', 0.31764706, 0.68627451, 0.89019608) ;
#20767 = CARTESIAN_POINT ( 'NONE',  ( 38.26194895904383486, -7.013682088886100452, 69.64448340153879258 ) ) ;
#20768 = ORIENTED_EDGE ( 'NONE', *, *, #14918, .F. ) ;
#20769 = CARTESIAN_POINT ( 'NONE',  ( 39.73277004305198545, -8.213682088886105959, 73.23812341099225875 ) ) ;
#20770 = VERTEX_POINT ( 'NONE', #17146 ) ;
#20771 = DIRECTION ( 'NONE',  ( 0.000000000000000000, 0.6568589528324746407, -0.7540134720837717852 ) ) ;
#20772 = VECTOR ( 'NONE', #19212, 1000.000000000000000 ) ;
#20773 = CARTESIAN_POINT ( 'NONE',  ( 39.37952058850012804, -15.00384086642191228, 71.78268878715390144 ) ) ;
#20774 = CARTESIAN_POINT ( 'NONE',  ( 33.31606138205700773, 3.392460599465057403, 64.84545171350526971 ) ) ;
#20775 = EDGE_CURVE ( 'NONE', #6643, #12177, #3600, .T. ) ;
#20776 = ORIENTED_EDGE ( 'NONE', *, *, #20106, .T. ) ;
#20777 = DIRECTION ( 'NONE',  ( -1.734723475976814737E-16, 0.000000000000000000, -1.000000000000000000 ) ) ;
#20778 = DIRECTION ( 'NONE',  ( -1.000000000000000000, 0.000000000000000000, 0.000000000000000000 ) ) ;
#20779 = CARTESIAN_POINT ( 'NONE',  ( 37.61123632939164452, -15.70384086642191157, 69.02690120949091579 ) ) ;
#20780 = CARTESIAN_POINT ( 'NONE',  ( 36.41626118072728246, -20.92798318178700612, 75.89274454529751779 ) ) ;
#20781 = CARTESIAN_POINT ( 'NONE',  ( 47.81606138205695089, -23.19619402982945644, 47.16846523730003327 ) ) ;
#20782 = CARTESIAN_POINT ( 'NONE',  ( 36.87297107704152666, -21.71368208888610951, 72.49904802271740323 ) ) ;
#20783 = DIRECTION ( 'NONE',  ( 0.000000000000000000, -3.491481338843135327E-15, -1.000000000000000000 ) ) ;
#20784 = DIRECTION ( 'NONE',  ( 1.000000000000000000, 2.999999999999999839E-15, 0.000000000000000000 ) ) ;
#20785 = ORIENTED_EDGE ( 'NONE', *, *, #11536, .F. ) ;
#20786 = PLANE ( 'NONE',  #17846 ) ;
#20787 = CARTESIAN_POINT ( 'NONE',  ( 33.40064408022072939, 41.43850569188389699, 79.37823623207322044 ) ) ;
#20788 = CARTESIAN_POINT ( 'NONE',  ( 40.14115730948191185, -7.103840866421910150, 71.43714994484034264 ) ) ;
#20789 = CIRCLE ( 'NONE', #2672, 1.550000000000002709 ) ;
#20790 = DIRECTION ( 'NONE',  ( 0.000000000000000000, 0.000000000000000000, 1.000000000000000000 ) ) ;
#20791 = LINE ( 'NONE', #3126, #5488 ) ;
#20792 = AXIS2_PLACEMENT_3D ( 'NONE', #23833, #22287, #10322 ) ;
#20793 = CARTESIAN_POINT ( 'NONE',  ( 37.80618814713140097, -23.91368208888610880, 73.13360434286902034 ) ) ;
#20794 = DIRECTION ( 'NONE',  ( 0.000000000000000000, -0.5735764363510444941, 0.8191520442889929088 ) ) ;
#20795 = CARTESIAN_POINT ( 'NONE',  ( 40.14115730948191185, -23.10384086642191193, 71.43714994484030001 ) ) ;
#20796 = LINE ( 'NONE', #1194, #16329 ) ;
#20797 = CARTESIAN_POINT ( 'NONE',  ( 39.29254315202756231, -26.81368208888610027, 69.94417936956671156 ) ) ;
#20798 = VERTEX_POINT ( 'NONE', #23054 ) ;
#20799 = ORIENTED_EDGE ( 'NONE', *, *, #9100, .T. ) ;
#20800 = DIRECTION ( 'NONE',  ( 0.000000000000000000, 0.3299742535180963943, -0.9439899321577402969 ) ) ;
#20801 = DIRECTION ( 'NONE',  ( 1.734723475976805122E-15, 2.999999999999999839E-15, 1.000000000000000000 ) ) ;
#20802 = CARTESIAN_POINT ( 'NONE',  ( 39.51027997493896748, 1.486317911113900658, 71.32335560751961623 ) ) ;
#20803 = CARTESIAN_POINT ( 'NONE',  ( 38.37017380507020192, -0.01368208888610084051, 72.51602215082118619 ) ) ;
#20804 = VERTEX_POINT ( 'NONE', #11096 ) ;
#20805 = EDGE_CURVE ( 'NONE', #16606, #23317, #1595, .T. ) ;
#20806 = ORIENTED_EDGE ( 'NONE', *, *, #6576, .F. ) ;
#20807 = DIRECTION ( 'NONE',  ( 1.000000000000000000, 0.000000000000000000, 0.000000000000000000 ) ) ;
#20808 = DIRECTION ( 'NONE',  ( -1.000000000000000000, 1.115179377413661005E-30, 3.717264591378870232E-16 ) ) ;
#20809 = EDGE_LOOP ( 'NONE', ( #24938, #15132, #19082, #8798, #6953 ) ) ;
#20810 = DIRECTION ( 'NONE',  ( -1.000000000000000000, -1.000000000000000078E-15, 0.000000000000000000 ) ) ;
#20811 = CARTESIAN_POINT ( 'NONE',  ( 37.80618814713138676, -3.703840866421904909, 69.62690120949091011 ) ) ;
#20812 = ADVANCED_FACE ( 'NONE', ( #12908 ), #7352, .F. ) ;
#20813 = CARTESIAN_POINT ( 'NONE',  ( 31.91606138205695231, 3.586515973360766996, -0.5067327973472466329 ) ) ;
#20814 = ORIENTED_EDGE ( 'NONE', *, *, #23554, .F. ) ;
#20815 = VERTEX_POINT ( 'NONE', #7096 ) ;
#20816 = DIRECTION ( 'NONE',  ( -1.000000000000000000, 0.000000000000000000, 0.000000000000000000 ) ) ;
#20817 = CARTESIAN_POINT ( 'NONE',  ( 39.98359781491296161, -4.413682088886105248, 71.86517103874048473 ) ) ;
#20818 = ORIENTED_EDGE ( 'NONE', *, *, #9414, .F. ) ;
#20819 = CARTESIAN_POINT ( 'NONE',  ( 36.64852494920107517, -26.20384086642191335, 71.86517103874047052 ) ) ;
#20820 = CARTESIAN_POINT ( 'NONE',  ( 40.31606138205700773, 39.69123852234597649, 69.30501292736988717 ) ) ;
#20821 = ORIENTED_EDGE ( 'NONE', *, *, #7774, .T. ) ;
#20822 = CARTESIAN_POINT ( 'NONE',  ( 43.13768477939176194, 2.905169009495293331, 6.099583767035779758 ) ) ;
#20823 = DIRECTION ( 'NONE',  ( -1.000000000000000000, 0.000000000000000000, 0.000000000000000000 ) ) ;
#20824 = CARTESIAN_POINT ( 'NONE',  ( 40.31606138205700773, 37.94123852234599781, 75.30501292736988717 ) ) ;
#20825 = LINE ( 'NONE', #14765, #4865 ) ;
#20826 = CARTESIAN_POINT ( 'NONE',  ( 43.81606138205700063, -37.81581049437287589, 70.47722359350073873 ) ) ;
#20827 = ORIENTED_EDGE ( 'NONE', *, *, #15560, .F. ) ;
#20828 = ORIENTED_EDGE ( 'NONE', *, *, #23665, .T. ) ;
#20830 = EDGE_CURVE ( 'NONE', #20166, #24103, #15199, .T. ) ;
#20829 = CARTESIAN_POINT ( 'NONE',  ( 30.81606138205700418, -34.55876147765410167, 70.30501292737000085 ) ) ;
#20831 = CARTESIAN_POINT ( 'NONE',  ( 32.81606138205700773, 22.19123852234699967, 69.30501292736994401 ) ) ;
#20832 = EDGE_CURVE ( 'NONE', #1739, #17171, #4954, .T. ) ;
#20833 = CARTESIAN_POINT ( 'NONE',  ( 39.51027997493896748, -14.51368208888610134, 71.32335560751960202 ) ) ;
#20834 = ORIENTED_EDGE ( 'NONE', *, *, #15258, .F. ) ;
#20835 = EDGE_CURVE ( 'NONE', #6972, #4199, #1656, .T. ) ;
#20836 = ORIENTED_EDGE ( 'NONE', *, *, #3487, .T. ) ;
#20837 = CARTESIAN_POINT ( 'NONE',  ( 36.31606138205698642, -9.092667827980706718, 28.75914562266559926 ) ) ;
#20838 = CARTESIAN_POINT ( 'NONE',  ( 37.25202387243752611, 0.7863179111138978161, 70.00779233799264034 ) ) ;
#20839 = CARTESIAN_POINT ( 'NONE',  ( 39.82603832034400426, -23.30384086642190766, 70.35351908239857721 ) ) ;
#20840 = LINE ( 'NONE', #14650, #8759 ) ;
#20841 = CARTESIAN_POINT ( 'NONE',  ( 36.29569395875879678, -7.313682088886101162, 69.98269868914869107 ) ) ;
#20842 = FACE_OUTER_BOUND ( 'NONE', #4545, .T. ) ;
#20843 = ORIENTED_EDGE ( 'NONE', *, *, #10358, .F. ) ;
#20844 = CARTESIAN_POINT ( 'NONE',  ( 36.31606138205700063, -31.05876147765400574, 73.55501292737010033 ) ) ;
#20845 = ADVANCED_FACE ( 'NONE', ( #13028 ), #18816, .F. ) ;
#20846 = LINE ( 'NONE', #1257, #3186 ) ;
#20847 = LINE ( 'NONE', #13123, #18612 ) ;
#20848 = CARTESIAN_POINT ( 'NONE',  ( 43.63145769492233228, 3.383950488897877307, 6.176937329184648995 ) ) ;
#20849 = DIRECTION ( 'NONE',  ( -1.000000000000000000, 0.000000000000000000, 0.000000000000000000 ) ) ;
#20850 = CYLINDRICAL_SURFACE ( 'NONE', #20526, 3.000000000000002665 ) ;
#20851 = ORIENTED_EDGE ( 'NONE', *, *, #19326, .T. ) ;
#20852 = DIRECTION ( 'NONE',  ( 0.000000000000000000, -0.5706330172266952383, 0.8212051873014186709 ) ) ;
#20853 = FACE_OUTER_BOUND ( 'NONE', #6684, .T. ) ;
#20854 = ORIENTED_EDGE ( 'NONE', *, *, #251, .T. ) ;
#20855 = VERTEX_POINT ( 'NONE', #5173 ) ;
#20856 = PRODUCT_DEFINITION_CONTEXT ( 'detailed design', #20659, 'design' ) ;
#20857 = CARTESIAN_POINT ( 'NONE',  ( 40.77203464402485622, -15.10384086642191548, 71.43714994484032843 ) ) ;
#20858 = CARTESIAN_POINT ( 'NONE',  ( 36.64852494920107517, -19.41368208888610525, 70.89533451361947414 ) ) ;
#20859 = CARTESIAN_POINT ( 'NONE',  ( 40.31606138205700773, -16.77230293220685198, 77.52306850662458260 ) ) ;
#20860 = SURFACE_STYLE_FILL_AREA ( #16736 ) ;
#20861 = ORIENTED_EDGE ( 'NONE', *, *, #24497, .T. ) ;
#20862 = CARTESIAN_POINT ( 'NONE',  ( 33.31606138205700773, -1.357181138186128067, 82.80501292736991559 ) ) ;
#20863 = DIRECTION ( 'NONE',  ( 0.000000000000000000, -1.000000000000000000, 6.938893903907221278E-15 ) ) ;
#20864 = CARTESIAN_POINT ( 'NONE',  ( 40.77203464402485622, -28.51368208888610667, 71.32335560751960202 ) ) ;
#20865 = AXIS2_PLACEMENT_3D ( 'NONE', #23119, #3425, #1981 ) ;
#20866 = EDGE_LOOP ( 'NONE', ( #20170, #20511 ) ) ;
#20867 = FILL_AREA_STYLE ('',( #8902 ) ) ;
#20868 = DIRECTION ( 'NONE',  ( -1.000000000000000000, 0.000000000000000000, 0.000000000000000000 ) ) ;
#20869 = CIRCLE ( 'NONE', #25367, 1.249999999999997780 ) ;
#20870 = TOROIDAL_SURFACE ( 'NONE', #3569, 1.800000000000000044, 0.2000000000000000111 ) ;
#20871 = CARTESIAN_POINT ( 'NONE',  ( 36.80608444377001121, -1.313682088886099386, 70.35351908239860563 ) ) ;
#20872 = DIRECTION ( 'NONE',  ( 0.000000000000000000, -0.3299742535180970049, 0.9439899321577400748 ) ) ;
#20873 = EDGE_CURVE ( 'NONE', #21126, #15455, #24625, .T. ) ;
#20874 = CARTESIAN_POINT ( 'NONE',  ( 39.82603832034401847, -22.31368208888610738, 72.40698646996131060 ) ) ;
#20875 = DIRECTION ( 'NONE',  ( -0.6606874543841287917, -0.6164467895351006810, -0.4283520086229165025 ) ) ;
#20876 = DIRECTION ( 'NONE',  ( 1.000000000000000000, 3.194449454093636459E-15, 9.596449257708877207E-17 ) ) ;
#20877 = CARTESIAN_POINT ( 'NONE',  ( 39.02742774030101458, -19.40384086642191264, 70.49320253461759478 ) ) ;
#20878 = CARTESIAN_POINT ( 'NONE',  ( 38.93415946300897446, -8.113682088886108090, 73.09843995877331224 ) ) ;
#20879 = ORIENTED_EDGE ( 'NONE', *, *, #650, .T. ) ;
#20880 = CARTESIAN_POINT ( 'NONE',  ( 41.81606138205687273, 42.19123852234595518, 61.80501292736988006 ) ) ;
#20881 = VERTEX_POINT ( 'NONE', #1291 ) ;
#20882 = CLOSED_SHELL ( 'NONE', ( #976, #283, #211, #8654, #22071, #7837, #21016, #2313, #12603, #12353, #21535, #3595, #4980, #22681, #9355, #23084, #15765, #18833, #1725, #7099, #6861, #3713, #19919, #20426, #5005, #11163, #5021, #20501, #10744, #2145, #19508, #13654, #7840, #3257, #2464, #25364, #5318, #7249, #22026, #2392, #5632, #19171 ) ) ;
#20883 = CARTESIAN_POINT ( 'NONE',  ( 39.95015449827720744, -5.003840866421912281, 71.96809898377888715 ) ) ;
#20884 = EDGE_CURVE ( 'NONE', #24591, #1030, #1533, .T. ) ;
#20885 = DIRECTION ( 'NONE',  ( -2.312964634635742267E-15, 0.8967398287344626739, 0.4425581086832399147 ) ) ;
#20886 = VECTOR ( 'NONE', #23327, 1000.000000000000000 ) ;
#20887 = VECTOR ( 'NONE', #1988, 1000.000000000000000 ) ;
#20888 = CARTESIAN_POINT ( 'NONE',  ( 36.64852494920107517, -1.413682088886102806, 70.89533451361948835 ) ) ;
#20889 = VERTEX_POINT ( 'NONE', #15074 ) ;
#20890 = CARTESIAN_POINT ( 'NONE',  ( 40.55423172469004811, -12.41368208888610525, 72.05058123536544201 ) ) ;
#20891 = VERTEX_POINT ( 'NONE', #22928 ) ;
#20892 = PLANE ( 'NONE',  #22234 ) ;
#20893 = EDGE_CURVE ( 'NONE', #21703, #22091, #9060, .T. ) ;
#20894 = CARTESIAN_POINT ( 'NONE',  ( 39.51027997493896748, -11.10384086642191015, 71.43714994484034264 ) ) ;
#20895 = EDGE_CURVE ( 'NONE', #9681, #22879, #732, .T. ) ;
#20896 = CARTESIAN_POINT ( 'NONE',  ( 40.31606138205700063, 5.191238522346998785, 68.80501292736998664 ) ) ;
#20897 = VERTEX_POINT ( 'NONE', #18041 ) ;
#20898 = LINE ( 'NONE', #5433, #22001 ) ;
#20899 = LINE ( 'NONE', #11113, #9225 ) ;
#20900 = CARTESIAN_POINT ( 'NONE',  ( 40.52078840805429394, -17.00384086642191406, 72.15350918040381600 ) ) ;
#20901 = CARTESIAN_POINT ( 'NONE',  ( 37.79585267494195477, -22.16015963634850650, 75.80517796092046012 ) ) ;
#20902 = DIRECTION ( 'NONE',  ( 0.000000000000000000, -0.8212051873014213355, -0.5706330172266915746 ) ) ;
#20903 = CARTESIAN_POINT ( 'NONE',  ( 36.64852494920107517, -21.41368208888610525, 70.89533451361947414 ) ) ;
#20904 = CARTESIAN_POINT ( 'NONE',  ( 32.81606138205700773, 2.191238522347000117, 69.30501292737000085 ) ) ;
#20905 = ADVANCED_FACE ( 'NONE', ( #7870 ), #3729, .F. ) ;
#20906 = PLANE ( 'NONE',  #17624 ) ;
#20907 = VECTOR ( 'NONE', #12477, 1000.000000000000000 ) ;
#20908 = ORIENTED_EDGE ( 'NONE', *, *, #16168, .F. ) ;
#20909 = VECTOR ( 'NONE', #19802, 1000.000000000000000 ) ;
#20910 = FACE_OUTER_BOUND ( 'NONE', #11731, .T. ) ;
#20911 = DIRECTION ( 'NONE',  ( 1.000000000000000000, 0.000000000000000000, 0.000000000000000000 ) ) ;
#20912 = CARTESIAN_POINT ( 'NONE',  ( 36.49096545463212493, -8.103840866421908373, 71.32335560751963044 ) ) ;
#20913 = APPLICATION_PROTOCOL_DEFINITION ( 'draft international standard', 'automotive_design', 1998, #2543 ) ;
#20914 = CARTESIAN_POINT ( 'NONE',  ( 45.81606138205700063, -25.52563857111379875, 92.39878177866870601 ) ) ;
#20915 = CARTESIAN_POINT ( 'NONE',  ( 39.95015449827720744, -26.61368208888610809, 70.79240656858104330 ) ) ;
#20916 = CARTESIAN_POINT ( 'NONE',  ( 45.81606138205695800, -0.7562224151693129892, -1.633662118351544734 ) ) ;
#20917 = CARTESIAN_POINT ( 'NONE',  ( 37.33957961208645315, -21.80384086642190766, 69.94417936956672577 ) ) ;
#20918 = CARTESIAN_POINT ( 'NONE',  ( 36.57819145821473228, -6.205787318996375035, 83.25770116091617012 ) ) ;
#20919 = CARTESIAN_POINT ( 'NONE',  ( 39.29254315202756231, -18.81368208888610027, 69.94417936956672577 ) ) ;
#20920 = ORIENTED_EDGE ( 'NONE', *, *, #4866, .F. ) ;
#20921 = CARTESIAN_POINT ( 'NONE',  ( 39.64521430340304420, -26.81368208888610738, 69.45876917294174291 ) ) ;
#20922 = ORIENTED_EDGE ( 'NONE', *, *, #11446, .T. ) ;
#20923 = DIRECTION ( 'NONE',  ( 1.734723475976814737E-16, -1.000000000000000000, 3.491481338843135327E-15 ) ) ;
#20924 = DIRECTION ( 'NONE',  ( 1.734723475976814737E-16, -1.000000000000000000, 3.491481338843135327E-15 ) ) ;
#20925 = CARTESIAN_POINT ( 'NONE',  ( 37.25260217561390874, 0.3863179111139002364, 71.78268878715394408 ) ) ;
#20926 = EDGE_CURVE ( 'NONE', #2906, #15674, #6187, .T. ) ;
#20927 = EDGE_CURVE ( 'NONE', #21068, #3466, #24244, .T. ) ;
#20928 = AXIS2_PLACEMENT_3D ( 'NONE', #966, #16695, #4728 ) ;
#20929 = ORIENTED_EDGE ( 'NONE', *, *, #11683, .T. ) ;
#20930 = ORIENTED_EDGE ( 'NONE', *, *, #7448, .T. ) ;
#20931 = FACE_OUTER_BOUND ( 'NONE', #1017, .T. ) ;
#20932 = CARTESIAN_POINT ( 'NONE',  ( 38.31606138205697931, -6.672912525257896021, -0.4345143786933236552 ) ) ;
#20933 = ORIENTED_EDGE ( 'NONE', *, *, #14372, .T. ) ;
#20934 = CARTESIAN_POINT ( 'NONE',  ( 39.95015449827720744, -7.003840866421910505, 71.96809898377888715 ) ) ;
#20935 = FACE_OUTER_BOUND ( 'NONE', #2277, .T. ) ;
#20936 = EDGE_CURVE ( 'NONE', #17636, #22981, #11998, .T. ) ;
#20937 = DIRECTION ( 'NONE',  ( -2.122643018205887308E-17, 1.000000000000000000, -3.120611096041553009E-15 ) ) ;
#20938 = VERTEX_POINT ( 'NONE', #23300 ) ;
#20939 = STYLED_ITEM ( 'NONE', ( #9847 ), #25444 ) ;
#20940 = VERTEX_POINT ( 'NONE', #15456 ) ;
#20941 = DIRECTION ( 'NONE',  ( -2.792262043613788535E-15, 0.8967398287344627850, 0.4425581086832399147 ) ) ;
#20942 = CARTESIAN_POINT ( 'NONE',  ( 36.68196826583682935, 0.3863179111138967392, 71.96809898377890136 ) ) ;
#20943 = CARTESIAN_POINT ( 'NONE',  ( 46.91606138205698073, -6.210967385200536484, -3.065230171572500772 ) ) ;
#20944 = CARTESIAN_POINT ( 'NONE',  ( 31.81606138205700418, -26.74044063519535186, 82.55501292737007191 ) ) ;
#20945 = VECTOR ( 'NONE', #9209, 1000.000000000000000 ) ;
#20946 =( BOUNDED_CURVE ( )  B_SPLINE_CURVE ( 3, ( #1911, #7864, #25349, #5661 ),
 .UNSPECIFIED., .F., .T. ) 
 B_SPLINE_CURVE_WITH_KNOTS ( ( 4, 4 ),
 ( 3.141592653589795336, 4.712388980384689674 ),
 .UNSPECIFIED. ) 
 CURVE ( )  GEOMETRIC_REPRESENTATION_ITEM ( )  RATIONAL_B_SPLINE_CURVE ( ( 1.000000000000000000, 0.8047378541243649375, 0.8047378541243649375, 1.000000000000000000 ) ) 
 REPRESENTATION_ITEM ( '' )  );
#20947 = ORIENTED_EDGE ( 'NONE', *, *, #3958, .F. ) ;
#20948 = DIRECTION ( 'NONE',  ( -1.000000000000000000, 0.000000000000000000, 0.000000000000000000 ) ) ;
#20949 = EDGE_CURVE ( 'NONE', #23854, #18988, #10058, .T. ) ;
#20950 = DIRECTION ( 'NONE',  ( 0.000000000000000000, -1.000000000000000000, 0.000000000000000000 ) ) ;
#20951 = CARTESIAN_POINT ( 'NONE',  ( 30.81606138205700418, 40.39281886181299797, 83.30501292736984453 ) ) ;
#20952 = CARTESIAN_POINT ( 'NONE',  ( 30.81606138205697931, -3.270329303098769014, -7.854091020184566396 ) ) ;
#20953 = FILL_AREA_STYLE ('',( #15694 ) ) ;
#20954 = VECTOR ( 'NONE', #4477, 1000.000000000000227 ) ;
#20955 = EDGE_LOOP ( 'NONE', ( #16473, #21642, #10062, #7213 ) ) ;
#20956 = CARTESIAN_POINT ( 'NONE',  ( 44.81606138205700063, -34.55876147765401640, 70.30501292737011454 ) ) ;
#20957 = ORIENTED_EDGE ( 'NONE', *, *, #1674, .F. ) ;
#20958 = ORIENTED_EDGE ( 'NONE', *, *, #2908, .F. ) ;
#20959 = DIRECTION ( 'NONE',  ( 0.000000000000000000, -9.938893903907220328E-15, -1.000000000000000000 ) ) ;
#20960 = CIRCLE ( 'NONE', #25026, 1.000000000000000888 ) ;
#20961 = DIRECTION ( 'NONE',  ( 0.000000000000000000, -1.000000000000000000, 2.999999999999999839E-15 ) ) ;
#20962 = CARTESIAN_POINT ( 'NONE',  ( 37.60469502381300089, -17.21368208888610241, 70.49320253461759478 ) ) ;
#20963 = ORIENTED_EDGE ( 'NONE', *, *, #4964, .T. ) ;
#20964 = ORIENTED_EDGE ( 'NONE', *, *, #23554, .T. ) ;
#20965 = CARTESIAN_POINT ( 'NONE',  ( 40.31606138205700773, 39.69123852234599781, 74.30501292736988717 ) ) ;
#20966 = CARTESIAN_POINT ( 'NONE',  ( 41.31606138205687273, 42.19123852234595518, 61.80501292736988006 ) ) ;
#20967 = CARTESIAN_POINT ( 'NONE',  ( 37.80618814713138676, -23.70384086642190979, 69.62690120949091011 ) ) ;
#20968 = VECTOR ( 'NONE', #1824, 1000.000000000000000 ) ;
#20969 = CARTESIAN_POINT ( 'NONE',  ( 31.81606138205700418, 28.12806996228107081, 65.30501292736992980 ) ) ;
#20970 = CARTESIAN_POINT ( 'NONE',  ( 40.26954217208371034, -4.713682088886099741, 69.89063713639259845 ) ) ;
#20971 = EDGE_LOOP ( 'NONE', ( #9774, #8588 ) ) ;
#20972 = CIRCLE ( 'NONE', #1225, 1.000000000000000888 ) ;
#20973 = EDGE_LOOP ( 'NONE', ( #18641, #20933, #5289, #20386 ) ) ;
#20974 = CARTESIAN_POINT ( 'NONE',  ( 39.82611197195675601, -5.886287209492222949, 83.28324666752695293 ) ) ;
#20975 = DIRECTION ( 'NONE',  ( -0.000000000000000000, 0.5735764363510463815, -0.8191520442889914655 ) ) ;
#20976 = EDGE_CURVE ( 'NONE', #19306, #3683, #7999, .T. ) ;
#20977 = LINE ( 'NONE', #15167, #18214 ) ;
#20978 = VECTOR ( 'NONE', #10534, 1000.000000000000227 ) ;
#20979 = EDGE_CURVE ( 'NONE', #21357, #24510, #7822, .T. ) ;
#20980 = CARTESIAN_POINT ( 'NONE',  ( 40.25357836725066818, -6.692310083303524060, 83.20492142726308771 ) ) ;
#20981 = CARTESIAN_POINT ( 'NONE',  ( 33.31606138205700773, 7.282926244446933595, 65.60596383066929604 ) ) ;
#20982 = CARTESIAN_POINT ( 'NONE',  ( 36.31606138205703616, 33.19123852234596939, 66.30501292736991559 ) ) ;
#20983 = ORIENTED_EDGE ( 'NONE', *, *, #18732, .T. ) ;
#20984 = DIRECTION ( 'NONE',  ( -1.000000000000000000, 0.000000000000000000, 0.000000000000000000 ) ) ;
#20985 = CARTESIAN_POINT ( 'NONE',  ( 41.06606138205698642, -9.092667827980692508, 28.75914562266559926 ) ) ;
#20986 = EDGE_LOOP ( 'NONE', ( #21855, #18643, #1313, #13206 ) ) ;
#20987 = ORIENTED_EDGE ( 'NONE', *, *, #16304, .F. ) ;
#20988 = CARTESIAN_POINT ( 'NONE',  ( 40.26954217208372455, -10.90384086642191974, 72.86986841596736042 ) ) ;
#20989 = VECTOR ( 'NONE', #23713, 1000.000000000000227 ) ;
#20990 = ADVANCED_FACE ( 'NONE', ( #8116 ), #9800, .F. ) ;
#20991 = FACE_OUTER_BOUND ( 'NONE', #2865, .T. ) ;
#20992 = CARTESIAN_POINT ( 'NONE',  ( 36.87297107704152666, -23.71368208888610951, 72.49904802271738902 ) ) ;
#20993 = VECTOR ( 'NONE', #15200, 1000.000000000000227 ) ;
#20994 =( BOUNDED_CURVE ( )  B_SPLINE_CURVE ( 3, ( #14317, #16622, #16491, #4533 ),
 .UNSPECIFIED., .F., .T. ) 
 B_SPLINE_CURVE_WITH_KNOTS ( ( 4, 4 ),
 ( 1.570796326794893227, 3.141592653589793116 ),
 .UNSPECIFIED. ) 
 CURVE ( )  GEOMETRIC_REPRESENTATION_ITEM ( )  RATIONAL_B_SPLINE_CURVE ( ( 1.000000000000000000, 0.8047378541243641603, 0.8047378541243641603, 1.000000000000000000 ) ) 
 REPRESENTATION_ITEM ( '' )  );
#20995 = ORIENTED_EDGE ( 'NONE', *, *, #16508, .T. ) ;
#20996 = DIRECTION ( 'NONE',  ( 1.047880217021202589E-15, -0.4425581086832399147, 0.8967398287344627850 ) ) ;
#20997 = LINE ( 'NONE', #19063, #24430 ) ;
#20998 = CARTESIAN_POINT ( 'NONE',  ( 40.33642880535524000, -20.31368208888610738, 72.77780686321126780 ) ) ;
#20999 = ORIENTED_EDGE ( 'NONE', *, *, #1598, .F. ) ;
#21000 = CARTESIAN_POINT ( 'NONE',  ( 38.82593461698262871, 1.086317911113899637, 69.62690120949091011 ) ) ;
#21001 = CARTESIAN_POINT ( 'NONE',  ( 30.81606138205697931, -4.589472609077253296, -6.350807634294812765 ) ) ;
#21002 = CARTESIAN_POINT ( 'NONE',  ( 40.14115730948191185, -14.51368208888610489, 71.32335560751960202 ) ) ;
#21003 = AXIS2_PLACEMENT_3D ( 'NONE', #12791, #21022, #5303 ) ;
#21004 = CARTESIAN_POINT ( 'NONE',  ( 40.31606138205700773, 37.94123852234599781, 74.30501292736988717 ) ) ;
#21005 = CARTESIAN_POINT ( 'NONE',  ( 38.41621794735363693, -36.60729675983900222, 84.30501292737011454 ) ) ;
#21006 = VECTOR ( 'NONE', #19294, 1000.000000000000000 ) ;
#21007 = CARTESIAN_POINT ( 'NONE',  ( 37.89291511884479036, -16.50384086642191050, 72.49843995877330372 ) ) ;
#21008 = CARTESIAN_POINT ( 'NONE',  ( 39.82603832034400426, -8.313682088886110932, 72.40698646996135324 ) ) ;
#21009 = VERTEX_POINT ( 'NONE', #25355 ) ;
#21010 = CARTESIAN_POINT ( 'NONE',  ( 38.31606138205700063, -22.22127907754186893, 75.30501292736998664 ) ) ;
#21011 = LINE ( 'NONE', #2862, #8232 ) ;
#21012 = VERTEX_POINT ( 'NONE', #21639 ) ;
#21013 = EDGE_LOOP ( 'NONE', ( #15016, #2643 ) ) ;
#21014 = CARTESIAN_POINT ( 'NONE',  ( 38.82593461698265003, -6.703840866421914235, 73.13360434286904876 ) ) ;
#21015 = CARTESIAN_POINT ( 'NONE',  ( 43.31606138205700063, 7.043113989679085307, 66.83274420321491505 ) ) ;
#21016 = ADVANCED_FACE ( 'NONE', ( #11867 ), #1886, .F. ) ;
#21017 = CARTESIAN_POINT ( 'NONE',  ( 36.80608444377001121, 0.6863179111138983934, 70.35351908239860563 ) ) ;
#21018 = EDGE_LOOP ( 'NONE', ( #7236, #4171, #11151, #5302 ) ) ;
#21019 = B_SPLINE_SURFACE_WITH_KNOTS ( 'NONE', 1, 3, ( 
 ( #20017, #19630, #6109, #9855 ),
 ( #43, #17714, #18098, #2355 ),
 ( #23992, #7924, #6370, #12301 ) ),
 .UNSPECIFIED., .F., .F., .F.,
 ( 2, 1, 2 ),
 ( 4, 4 ),
 ( -0.01000000000000000021, 0.000000000000000000, 1.000000000000000000 ),
 ( 0.000000000000000000, 1.000000000000000000 ),
 .UNSPECIFIED. ) ;
#21020 = CARTESIAN_POINT ( 'NONE',  ( 40.55423172469004811, -6.413682088886103472, 72.05058123536544201 ) ) ;
#21021 = ORIENTED_EDGE ( 'NONE', *, *, #22216, .F. ) ;
#21022 = DIRECTION ( 'NONE',  ( -1.000000000000000000, 1.040834085586084551E-30, 3.469446951953615175E-16 ) ) ;
#21023 = CARTESIAN_POINT ( 'NONE',  ( 38.26194895904384197, -2.603840866421912814, 72.51602215082118619 ) ) ;
#21024 = CARTESIAN_POINT ( 'NONE',  ( 36.31606138205700063, -4.357181138186127178, 82.80501292736992980 ) ) ;
#21025 = VECTOR ( 'NONE', #11816, 1000.000000000000000 ) ;
#21026 = EDGE_LOOP ( 'NONE', ( #2053, #17351, #9637, #7920 ) ) ;
#21027 = FACE_OUTER_BOUND ( 'NONE', #89, .T. ) ;
#21028 = DIRECTION ( 'NONE',  ( 1.000000000000000000, 1.734723475976804876E-16, -1.734723475976814737E-16 ) ) ;
#21029 = CARTESIAN_POINT ( 'NONE',  ( 38.26194895904384197, -18.60384086642191548, 73.71602215082113219 ) ) ;
#21030 = VECTOR ( 'NONE', #6652, 1000.000000000000000 ) ;
#21031 = CARTESIAN_POINT ( 'NONE',  ( 36.41626118072728246, -20.85922748787637815, 75.39235863515375513 ) ) ;
#21032 = DIRECTION ( 'NONE',  ( 0.000000000000000000, 0.000000000000000000, -1.000000000000000000 ) ) ;
#21033 = CARTESIAN_POINT ( 'NONE',  ( 39.75915168707250302, -20.71368208888610596, 70.26145752964251301 ) ) ;
#21034 = CARTESIAN_POINT ( 'NONE',  ( 35.91606138205695942, 0.5799492015812600654, -3.145019409304214530 ) ) ;
#21035 = CARTESIAN_POINT ( 'NONE',  ( 43.31606138205700063, -20.45664737071796324, 43.87694304485803798 ) ) ;
#21036 = VERTEX_POINT ( 'NONE', #18167 ) ;
#21037 = CYLINDRICAL_SURFACE ( 'NONE', #2561, 1.000000000000000888 ) ;
#21038 = DIRECTION ( 'NONE',  ( 1.734723475976814737E-16, -1.000000000000000000, 3.491481338843135327E-15 ) ) ;
#21039 = CARTESIAN_POINT ( 'NONE',  ( 36.64852494920107517, -6.203840866421912459, 71.86517103874049894 ) ) ;
#21040 = PRODUCT_CONTEXT ( 'NONE', #17055, 'mechanical' ) ;
#21041 = FACE_OUTER_BOUND ( 'NONE', #5229, .T. ) ;
#21042 = CARTESIAN_POINT ( 'NONE',  ( 37.33957961208646736, -23.81368208888611093, 72.81632618279320468 ) ) ;
#21043 = FACE_OUTER_BOUND ( 'NONE', #22084, .T. ) ;
#21044 = VECTOR ( 'NONE', #21601, 1000.000000000000000 ) ;
#21045 = CARTESIAN_POINT ( 'NONE',  ( 39.75915168707251723, -22.90384086642190908, 72.49904802271738902 ) ) ;
#21046 = CARTESIAN_POINT ( 'NONE',  ( 36.99159426505191561, -5.676177574760129296, 82.79426834405568059 ) ) ;
#21047 = ADVANCED_FACE ( 'NONE', ( #2427 ), #12625, .T. ) ;
#21048 =( GEOMETRIC_REPRESENTATION_CONTEXT ( 3 ) GLOBAL_UNCERTAINTY_ASSIGNED_CONTEXT ( ( #22087 ) ) GLOBAL_UNIT_ASSIGNED_CONTEXT ( ( #7632, #17549, #13933 ) ) REPRESENTATION_CONTEXT ( 'NONE', 'WORKASPACE' ) );
#21049 = CARTESIAN_POINT ( 'NONE',  ( 39.98359781491296161, -16.41368208888610525, 71.86517103874047052 ) ) ;
#21050 = ORIENTED_EDGE ( 'NONE', *, *, #7275, .F. ) ;
#21051 = CARTESIAN_POINT ( 'NONE',  ( 40.52078840805429394, 0.9961591335780859424, 72.15350918040385864 ) ) ;
#21052 = ORIENTED_EDGE ( 'NONE', *, *, #25469, .F. ) ;
#21053 = DIRECTION ( 'NONE',  ( 2.156013462999745228E-15, -1.000000000000000000, 3.491481338843135327E-15 ) ) ;
#21054 = CARTESIAN_POINT ( 'NONE',  ( 40.31606138205701484, -19.40517585842702175, 23.66972737280834238 ) ) ;
#21055 = CARTESIAN_POINT ( 'NONE',  ( 37.31647492878124694, -24.30384086642191122, 72.03616607671141026 ) ) ;
#21056 = ORIENTED_EDGE ( 'NONE', *, *, #4286, .F. ) ;
#21057 = ORIENTED_EDGE ( 'NONE', *, *, #23142, .F. ) ;
#21058 = LINE ( 'NONE', #3401, #2218 ) ;
#21059 = CARTESIAN_POINT ( 'NONE',  ( 43.81606138205700063, 28.12806996228107437, 66.30501292736992980 ) ) ;
#21060 = ORIENTED_EDGE ( 'NONE', *, *, #4286, .T. ) ;
#21061 = CARTESIAN_POINT ( 'NONE',  ( 33.40064408022072939, 42.57231754924293909, 79.57823623207322328 ) ) ;
#21062 = CARTESIAN_POINT ( 'NONE',  ( 36.49096545463212493, -2.103840866421912814, 71.32335560751963044 ) ) ;
#21063 = CARTESIAN_POINT ( 'NONE',  ( 33.31606138205700773, -18.80550481115971806, 25.27912300651437150 ) ) ;
#21064 = CARTESIAN_POINT ( 'NONE',  ( 35.91606138205695942, -0.07962245140795930209, -2.393377716359348817 ) ) ;
#21065 = VECTOR ( 'NONE', #9664, 1000.000000000000227 ) ;
#21066 = ORIENTED_EDGE ( 'NONE', *, *, #23336, .T. ) ;
#21067 = EDGE_CURVE ( 'NONE', #23614, #22308, #20086, .T. ) ;
#21068 = VERTEX_POINT ( 'NONE', #8376 ) ;
#21069 = DIRECTION ( 'NONE',  ( 0.000000000000000000, -1.000000000000000000, 3.469446951953617344E-15 ) ) ;
#21070 = EDGE_CURVE ( 'NONE', #8317, #16702, #11109, .T. ) ;
#21071 = CARTESIAN_POINT ( 'NONE',  ( 36.87297107704153376, -1.713682088886107957, 72.49904802271743165 ) ) ;
#21072 = VECTOR ( 'NONE', #975, 1000.000000000000000 ) ;
#21073 = CARTESIAN_POINT ( 'NONE',  ( 37.33957961208645315, -25.80384086642190766, 69.94417936956671156 ) ) ;
#21074 = ADVANCED_FACE ( 'NONE', ( #14292 ), #22141, .F. ) ;
#21075 = DIRECTION ( 'NONE',  ( 1.734723475976804876E-16, 3.496552006265755350E-15, 1.000000000000000000 ) ) ;
#21076 = ADVANCED_FACE ( 'NONE', ( #22269 ), #2677, .F. ) ;
#21077 = ADVANCED_FACE ( 'NONE', ( #13258 ), #9394, .T. ) ;
#21078 = EDGE_LOOP ( 'NONE', ( #16228, #24561, #1802, #3544 ) ) ;
#21079 = CARTESIAN_POINT ( 'NONE',  ( 36.31606138205700063, 5.691238522346998785, 68.80501292736998664 ) ) ;
#21080 = CARTESIAN_POINT ( 'NONE',  ( 30.81606138205706813, -35.90387122078356441, 69.64117576433150703 ) ) ;
#21081 = DIRECTION ( 'NONE',  ( 4.341746501209495972E-16, -0.4341746501209495790, -0.9008287146801833289 ) ) ;
#21082 = ORIENTED_EDGE ( 'NONE', *, *, #8639, .T. ) ;
#21083 = PLANE ( 'NONE',  #4167 ) ;
#21084 = VERTEX_POINT ( 'NONE', #24939 ) ;
#21085 = ORIENTED_EDGE ( 'NONE', *, *, #11478, .T. ) ;
#21086 = EDGE_CURVE ( 'NONE', #9087, #12177, #8224, .T. ) ;
#21087 = CARTESIAN_POINT ( 'NONE',  ( 33.31606138205700773, -10.93995761290683255, 80.99653337025984001 ) ) ;
#21088 = DIRECTION ( 'NONE',  ( -1.000000000000000000, 0.000000000000000000, 0.000000000000000000 ) ) ;
#21089 = CARTESIAN_POINT ( 'NONE',  ( 39.37952058850012804, -16.61368208888610098, 70.97781676520601479 ) ) ;
#21090 = ORIENTED_EDGE ( 'NONE', *, *, #5941, .T. ) ;
#21091 = VERTEX_POINT ( 'NONE', #15046 ) ;
#21092 = VECTOR ( 'NONE', #8582, 1000.000000000000000 ) ;
#21093 = FACE_BOUND ( 'NONE', #6924, .T. ) ;
#21094 = CARTESIAN_POINT ( 'NONE',  ( 40.31606138205701484, -20.02093502212014897, 26.61211107664843212 ) ) ;
#21095 = CARTESIAN_POINT ( 'NONE',  ( 37.69796330110505522, -26.50384086642190695, 73.09843995877328382 ) ) ;
#21096 = LINE ( 'NONE', #9381, #21887 ) ;
#21097 = ADVANCED_FACE ( 'NONE', ( #17122 ), #13003, .F. ) ;
#21098 = VECTOR ( 'NONE', #13524, 1000.000000000000000 ) ;
#21099 = AXIS2_PLACEMENT_3D ( 'NONE', #14903, #18647, #10548 ) ;
#21100 = ORIENTED_EDGE ( 'NONE', *, *, #22176, .F. ) ;
#21101 = CARTESIAN_POINT ( 'NONE',  ( 40.31606138205700063, 5.691238522346989903, 65.80501292736998664 ) ) ;
#21102 = LINE ( 'NONE', #19041, #16344 ) ;
#21103 = AXIS2_PLACEMENT_3D ( 'NONE', #15645, #9736, #23243 ) ;
#21104 = DIRECTION ( 'NONE',  ( -2.048868001712899108E-15, 0.6595716529892353686, -0.7516416929448815898 ) ) ;
#21105 = CARTESIAN_POINT ( 'NONE',  ( 38.44711690269065940, -5.204193249396277032, 83.31006292736994112 ) ) ;
#21106 = DIRECTION ( 'NONE',  ( 1.022195611122249672E-16, -0.1771812806364704007, -0.9841782327363373106 ) ) ;
#21107 = AXIS2_PLACEMENT_3D ( 'NONE', #3914, #9721, #7657 ) ;
#21108 = DIRECTION ( 'NONE',  ( 0.000000000000000000, 1.000000000000000000, 0.000000000000000000 ) ) ;
#21109 = ORIENTED_EDGE ( 'NONE', *, *, #24744, .T. ) ;
#21110 = CARTESIAN_POINT ( 'NONE',  ( 33.31606138205700773, -27.52349462642295208, 56.67559192035834315 ) ) ;
#21111 = AXIS2_PLACEMENT_3D ( 'NONE', #17619, #9645, #5892 ) ;
#21112 = CARTESIAN_POINT ( 'NONE',  ( 35.31606138205700773, 8.104266321858618838, 55.82104096753806033 ) ) ;
#21113 = ORIENTED_EDGE ( 'NONE', *, *, #19649, .T. ) ;
#21114 = VERTEX_POINT ( 'NONE', #21110 ) ;
#21115 = UNCERTAINTY_MEASURE_WITH_UNIT (LENGTH_MEASURE( 1.000000000000000082E-05 ), #22616, 'distance_accuracy_value', 'NONE');
#21116 = CARTESIAN_POINT ( 'NONE',  ( 36.11133435605973574, -10.00384086642191761, 70.60699637195612866 ) ) ;
#21117 = AXIS2_PLACEMENT_3D ( 'NONE', #18204, #8541, #16127 ) ;
#21118 = DIRECTION ( 'NONE',  ( 1.836970198721029688E-16, 2.999999999999999839E-15, 1.000000000000000000 ) ) ;
#21119 = CARTESIAN_POINT ( 'NONE',  ( 38.37017380507020192, -18.01368208888611022, 73.11602215082116629 ) ) ;
#21120 = AXIS2_PLACEMENT_3D ( 'NONE', #519, #19733, #14 ) ;
#21121 = ORIENTED_EDGE ( 'NONE', *, *, #20422, .F. ) ;
#21122 = CARTESIAN_POINT ( 'NONE',  ( 45.81606138205700063, -3.831401139557048197, 80.75501292737000369 ) ) ;
#21123 = DIRECTION ( 'NONE',  ( 1.000000000000000000, 0.000000000000000000, 0.000000000000000000 ) ) ;
#21124 = CIRCLE ( 'NONE', #2603, 3.999999999999996447 ) ;
#21125 = CARTESIAN_POINT ( 'NONE',  ( 36.89935272106204422, -23.21368208888610241, 69.52238214136765748 ) ) ;
#21126 = VERTEX_POINT ( 'NONE', #1394 ) ;
#21127 = DIRECTION ( 'NONE',  ( 0.000000000000000000, 1.000000000000000000, -3.469446951953613400E-15 ) ) ;
#21128 = DIRECTION ( 'NONE',  ( 2.595751990468335074E-30, 1.000000000000000000, -3.491481338843135327E-15 ) ) ;
#21129 = AXIS2_PLACEMENT_3D ( 'NONE', #9729, #3534, #1474 ) ;
#21130 = COLOUR_RGB ( '', 0.40784314, 0.44705882, 0.49803922) ;
#21131 = CARTESIAN_POINT ( 'NONE',  ( 36.31606138205700063, -16.48551471403133206, 77.11349248448009064 ) ) ;
#21132 = AXIS2_PLACEMENT_3D ( 'NONE', #3987, #16084, #13657 ) ;
#21133 = CARTESIAN_POINT ( 'NONE',  ( 36.31606138205700063, -6.942307388142325841, 83.16359031225202614 ) ) ;
#21134 = CARTESIAN_POINT ( 'NONE',  ( 39.37952058850012804, -15.00384086642191228, 71.78268878715390144 ) ) ;
#21135 = CARTESIAN_POINT ( 'NONE',  ( 39.82603832034400426, -0.3136820888861094336, 72.40698646996135324 ) ) ;
#21136 = ORIENTED_EDGE ( 'NONE', *, *, #20420, .T. ) ;
#21137 = CARTESIAN_POINT ( 'NONE',  ( 43.06606138205700063, 41.44123852234599070, 73.55501292736987295 ) ) ;
#21138 = CIRCLE ( 'NONE', #5493, 1.000000000000000000 ) ;
#21139 = DIRECTION ( 'NONE',  ( 1.000000000000000000, 2.440719103442460911E-15, 1.328886038262200866E-15 ) ) ;
#21140 = ORIENTED_EDGE ( 'NONE', *, *, #593, .F. ) ;
#21141 = EDGE_LOOP ( 'NONE', ( #11011, #16898, #10352, #6002 ) ) ;
#21143 =( BOUNDED_CURVE ( )  B_SPLINE_CURVE ( 3, ( #22214, #20292, #2627, #2742 ),
 .UNSPECIFIED., .F., .T. ) 
 B_SPLINE_CURVE_WITH_KNOTS ( ( 4, 4 ),
 ( 1.570796326794895004, 3.141592653589795336 ),
 .UNSPECIFIED. ) 
 CURVE ( )  GEOMETRIC_REPRESENTATION_ITEM ( )  RATIONAL_B_SPLINE_CURVE ( ( 1.000000000000000000, 0.8047378541243649375, 0.8047378541243649375, 1.000000000000000000 ) ) 
 REPRESENTATION_ITEM ( '' )  );
#21142 = CARTESIAN_POINT ( 'NONE',  ( 39.02088643472237806, -28.70384086642191690, 73.73360434286898624 ) ) ;
#21144 = CARTESIAN_POINT ( 'NONE',  ( 36.49096545463212493, -1.513682088886105559, 71.43714994484035685 ) ) ;
#21145 = CARTESIAN_POINT ( 'NONE',  ( 40.26954217208371034, -2.713682088886101962, 69.89063713639259845 ) ) ;
#21146 = ORIENTED_EDGE ( 'NONE', *, *, #7061, .T. ) ;
#21147 = DIRECTION ( 'NONE',  ( -1.849283715844614702E-16, 0.8212051873014210024, 0.5706330172266920187 ) ) ;
#21148 = ADVANCED_FACE ( 'NONE', ( #3324 ), #11065, .F. ) ;
#21149 = CARTESIAN_POINT ( 'NONE',  ( 38.00113996487112189, -5.703840866421911571, 70.22690120949091863 ) ) ;
#21150 = EDGE_CURVE ( 'NONE', #17655, #2946, #7325, .T. ) ;
#21151 = PLANE ( 'NONE',  #23329 ) ;
#21152 = ORIENTED_EDGE ( 'NONE', *, *, #1979, .T. ) ;
#21153 = DIRECTION ( 'NONE',  ( -0.9681609007195522976, 0.2503287245161955887, -7.060689259245944321E-16 ) ) ;
#21154 = FACE_OUTER_BOUND ( 'NONE', #11180, .T. ) ;
#21155 = CARTESIAN_POINT ( 'NONE',  ( 40.55423172469004101, -7.203840866421916900, 70.70992431699450265 ) ) ;
#21156 = AXIS2_PLACEMENT_3D ( 'NONE', #10125, #14242, #16282 ) ;
#21157 = CARTESIAN_POINT ( 'NONE',  ( 36.72121174906109786, -21.43480018258233954, 75.33032012337542938 ) ) ;
#21158 = LINE ( 'NONE', #21658, #5007 ) ;
#21159 = CARTESIAN_POINT ( 'NONE',  ( 36.49096545463212493, -11.51368208888609956, 71.43714994484034264 ) ) ;
#21160 = DIRECTION ( 'NONE',  ( 2.011972697750610993E-15, -0.6595716529892349245, 0.7516416929448819229 ) ) ;
#21161 = AXIS2_PLACEMENT_3D ( 'NONE', #8458, #4716, #24397 ) ;
#21162 = DIRECTION ( 'NONE',  ( 3.469446951953614189E-15, -0.8967398287344635621, -0.4425581086832386379 ) ) ;
#21163 = ORIENTED_EDGE ( 'NONE', *, *, #9353, .T. ) ;
#21164 = DIRECTION ( 'NONE',  ( 1.000000000000000000, 0.000000000000000000, 0.000000000000000000 ) ) ;
#21165 = ADVANCED_FACE ( 'NONE', ( #18923 ), #7453, .T. ) ;
#21166 = CARTESIAN_POINT ( 'NONE',  ( 38.26194895904384907, -6.603840866421916367, 73.11602215082118050 ) ) ;
#21167 = PRODUCT_CONTEXT ( 'NONE', #24577, 'mechanical' ) ;
#21168 = FACE_OUTER_BOUND ( 'NONE', #6416, .T. ) ;
#21169 = CARTESIAN_POINT ( 'NONE',  ( 39.98359781491296161, -16.41368208888610525, 71.86517103874047052 ) ) ;
#21170 = PRODUCT_DEFINITION_FORMATION_WITH_SPECIFIED_SOURCE ( 'ANY', '', #9311, .NOT_KNOWN. ) ;
#21171 = CARTESIAN_POINT ( 'NONE',  ( 43.81606138205700063, 3.172506336381830661, 12.50058896911730066 ) ) ;
#21172 = AXIS2_PLACEMENT_3D ( 'NONE', #13829, #9472, #25399 ) ;
#21173 = CARTESIAN_POINT ( 'NONE',  ( 39.29254315202757653, -16.80384086642191477, 72.81632618279321889 ) ) ;
#21174 = CARTESIAN_POINT ( 'NONE',  ( 36.57819145821473228, -6.206269038048873199, 83.26272840620944748 ) ) ;
#21175 = CARTESIAN_POINT ( 'NONE',  ( 38.93415946300897446, -20.11368208888610809, 73.09843995877329803 ) ) ;
#21176 = ORIENTED_EDGE ( 'NONE', *, *, #1180, .T. ) ;
#21177 = CARTESIAN_POINT ( 'NONE',  ( 36.98690846071097837, -27.81368208888610738, 73.30173637941817333 ) ) ;
#21178 = ORIENTED_EDGE ( 'NONE', *, *, #20761, .F. ) ;
#21179 = CARTESIAN_POINT ( 'NONE',  ( 43.31606138205700063, -13.04008168869994222, 21.66778101221729713 ) ) ;
#21180 = AXIS2_PLACEMENT_3D ( 'NONE', #15221, #22700, #20783 ) ;
#21181 = DIRECTION ( 'NONE',  ( 0.000000000000000000, 0.3299742535180974490, -0.9439899321577398528 ) ) ;
#21182 = CARTESIAN_POINT ( 'NONE',  ( 38.93987200065210175, -22.80384086642191122, 72.33091598616826445 ) ) ;
#21183 = ORIENTED_EDGE ( 'NONE', *, *, #4197, .T. ) ;
#21184 = VERTEX_POINT ( 'NONE', #13388 ) ;
#21185 = DIRECTION ( 'NONE',  ( 0.000000000000000000, 1.000000000000000000, 0.000000000000000000 ) ) ;
#21186 = CARTESIAN_POINT ( 'NONE',  ( 41.81606138205687273, 42.19123852234595518, 61.30501292736988006 ) ) ;
#21187 = EDGE_LOOP ( 'NONE', ( #4261, #3978, #8828, #14153 ) ) ;
#21188 = DIRECTION ( 'NONE',  ( 0.000000000000000000, 0.000000000000000000, -1.000000000000000000 ) ) ;
#21189 = CARTESIAN_POINT ( 'NONE',  ( 40.55423172469004101, -27.20384086642191690, 70.70992431699446001 ) ) ;
#21190 = CARTESIAN_POINT ( 'NONE',  ( 29.81606138205707524, -38.13418765192407989, 68.51141129791366780 ) ) ;
#21191 = LINE ( 'NONE', #7413, #712 ) ;
#21192 = CIRCLE ( 'NONE', #8030, 0.7500000000000006661 ) ;
#21193 = ORIENTED_EDGE ( 'NONE', *, *, #14064, .T. ) ;
#21194 = ORIENTED_EDGE ( 'NONE', *, *, #22369, .F. ) ;
#21195 = CARTESIAN_POINT ( 'NONE',  ( 40.81606138205700773, -31.05876147765399864, 75.30501292737010033 ) ) ;
#21196 = DIRECTION ( 'NONE',  ( 0.000000000000000000, 0.7540134720837716742, 0.6568589528324746407 ) ) ;
#21197 = CARTESIAN_POINT ( 'NONE',  ( 38.93415946300897446, -25.50384086642190695, 69.66206559358661821 ) ) ;
#21198 = DIRECTION ( 'NONE',  ( 0.000000000000000000, 0.5706330172266952383, -0.8212051873014186709 ) ) ;
#21199 = EDGE_LOOP ( 'NONE', ( #21336, #12357, #10790, #6887 ) ) ;
#21200 = CARTESIAN_POINT ( 'NONE',  ( 2.230251030284979743E-14, -7.197381196808558812, -3.552044091124126890 ) ) ;
#21201 = FACE_OUTER_BOUND ( 'NONE', #1900, .T. ) ;
#21202 = PLANE ( 'NONE',  #7706 ) ;
#21203 = VERTEX_POINT ( 'NONE', #15173 ) ;
#21204 = DIRECTION ( 'NONE',  ( -1.000000000000000000, -1.159780179694326360E-16, -8.617271610285116919E-17 ) ) ;
#21205 = ORIENTED_EDGE ( 'NONE', *, *, #243, .T. ) ;
#21206 = ORIENTED_EDGE ( 'NONE', *, *, #10888, .F. ) ;
#21207 = VECTOR ( 'NONE', #14670, 1000.000000000000000 ) ;
#21208 = FACE_OUTER_BOUND ( 'NONE', #20089, .T. ) ;
#21209 = CARTESIAN_POINT ( 'NONE',  ( 39.37952058850012804, -12.61368208888609921, 70.97781676520601479 ) ) ;
#21210 = EDGE_CURVE ( 'NONE', #6943, #25358, #23028, .T. ) ;
#21211 = CARTESIAN_POINT ( 'NONE',  ( 37.89291511884476904, -9.113682088886102761, 70.26206559358664094 ) ) ;
#21212 = ORIENTED_EDGE ( 'NONE', *, *, #19961, .T. ) ;
#21213 = ORIENTED_EDGE ( 'NONE', *, *, #5307, .T. ) ;
#21214 = DIRECTION ( 'NONE',  ( -1.327674326049719602E-15, 0.4425581086832399147, -0.8967398287344627850 ) ) ;
#21215 = VERTEX_POINT ( 'NONE', #21233 ) ;
#21216 = CARTESIAN_POINT ( 'NONE',  ( 39.95015449827720744, 1.386317911113894130, 70.79240656858108593 ) ) ;
#21217 = CARTESIAN_POINT ( 'NONE',  ( 36.87297107704149823, -17.90384086642190908, 70.26145752964252722 ) ) ;
#21218 = EDGE_CURVE ( 'NONE', #9369, #10963, #18789, .T. ) ;
#21219 = EDGE_CURVE ( 'NONE', #17655, #22871, #3456, .T. ) ;
#21220 = EDGE_CURVE ( 'NONE', #10160, #2724, #19172, .T. ) ;
#21221 = CARTESIAN_POINT ( 'NONE',  ( 42.99772342963552774, 2.840642293467601665, 6.103164780676344492 ) ) ;
#21222 = CARTESIAN_POINT ( 'NONE',  ( 39.02742774030102879, -18.21368208888610241, 72.26730301774234988 ) ) ;
#21223 = ORIENTED_EDGE ( 'NONE', *, *, #17303, .F. ) ;
#21224 = CARTESIAN_POINT ( 'NONE',  ( 32.81606138205700773, 2.191238522347000117, 69.30501292737000085 ) ) ;
#21225 = EDGE_CURVE ( 'NONE', #23789, #23772, #14795, .T. ) ;
#21226 = DIRECTION ( 'NONE',  ( -1.000000000000000000, 6.018531076210120799E-31, 1.734723475976804876E-16 ) ) ;
#21227 = EDGE_CURVE ( 'NONE', #18113, #18276, #5006, .T. ) ;
#21228 = DIRECTION ( 'NONE',  ( 0.000000000000000000, -1.000000000000000000, 2.999999999999999839E-15 ) ) ;
#21229 = CARTESIAN_POINT ( 'NONE',  ( 39.82611197195675601, -5.886615264206325193, 83.28828619899245211 ) ) ;
#21230 = DIRECTION ( 'NONE',  ( -1.327674326049719602E-15, 0.4425581086832399147, -0.8967398287344627850 ) ) ;
#21231 = CARTESIAN_POINT ( 'NONE',  ( 44.06606138205700063, 40.39281886181299797, 82.55501292736983032 ) ) ;
#21232 = VERTEX_POINT ( 'NONE', #12876 ) ;
#21233 = CARTESIAN_POINT ( 'NONE',  ( 40.31606138205702194, -21.37925193044962313, 31.05911325134166034 ) ) ;
#21234 = CARTESIAN_POINT ( 'NONE',  ( 31.81606138205700418, -26.74044063519544778, 66.30501292737000085 ) ) ;
#21235 = VERTEX_POINT ( 'NONE', #3064 ) ;
#21236 = ORIENTED_EDGE ( 'NONE', *, *, #6319, .T. ) ;
#21237 = CARTESIAN_POINT ( 'NONE',  ( 40.52078840805429394, -9.003840866421915834, 72.15350918040385864 ) ) ;
#21238 = CARTESIAN_POINT ( 'NONE',  ( 38.31606138205687984, 42.19123852234596939, 65.30501292736988717 ) ) ;
#21239 = CARTESIAN_POINT ( 'NONE',  ( 37.33957961208646736, -15.81368208888610916, 72.81632618279321889 ) ) ;
#21240 = EDGE_CURVE ( 'NONE', #16610, #22911, #10939, .T. ) ;
#21241 = EDGE_CURVE ( 'NONE', #18444, #4444, #8650, .T. ) ;
#21242 =( LENGTH_UNIT ( ) NAMED_UNIT ( * ) SI_UNIT ( .MILLI., .METRE. ) );
#21243 = ORIENTED_EDGE ( 'NONE', *, *, #2001, .F. ) ;
#21244 = DIRECTION ( 'NONE',  ( 1.327674326049719602E-15, -0.4425581086832399147, 0.8967398287344627850 ) ) ;
#21245 = DIRECTION ( 'NONE',  ( 6.195440985631459015E-17, 1.000000000000000000, -2.999999999999999839E-15 ) ) ;
#21246 = CARTESIAN_POINT ( 'NONE',  ( 39.12911128074873801, -20.11368208888610809, 73.69843995877327814 ) ) ;
#21247 = ORIENTED_EDGE ( 'NONE', *, *, #15612, .T. ) ;
#21248 = CARTESIAN_POINT ( 'NONE',  ( 45.06606138205697221, -5.022037326221688858, -5.474317061061731771 ) ) ;
#21249 = CARTESIAN_POINT ( 'NONE',  ( 40.31606138205700773, 39.69123852234599781, 74.30501292736988717 ) ) ;
#21250 = ADVANCED_FACE ( 'NONE', ( #7204 ), #22902, .F. ) ;
#21251 = LINE ( 'NONE', #9795, #22576 ) ;
#21252 = DIRECTION ( 'NONE',  ( 1.000000000000000000, 0.000000000000000000, 0.000000000000000000 ) ) ;
#21253 = CARTESIAN_POINT ( 'NONE',  ( 37.12184278917507640, -14.10384086642191370, 71.32335560751961623 ) ) ;
#21254 = CARTESIAN_POINT ( 'NONE',  ( 38.82593461698262871, -0.9136820888861022505, 69.62690120949091011 ) ) ;
#21255 = ORIENTED_EDGE ( 'NONE', *, *, #3584, .T. ) ;
#21256 = CARTESIAN_POINT ( 'NONE',  ( 32.81606138205700773, -37.53049398575952722, 70.06662099985001646 ) ) ;
#21257 = ADVANCED_FACE ( 'NONE', ( #19906 ), #18109, .F. ) ;
#21258 = CARTESIAN_POINT ( 'NONE',  ( 29.71606138205696368, 0.8576245772853353655, -1.570935883000529332 ) ) ;
#21259 = EDGE_LOOP ( 'NONE', ( #10693, #18119, #18938, #1576 ) ) ;
#21260 = ORIENTED_EDGE ( 'NONE', *, *, #16090, .F. ) ;
#21261 = CARTESIAN_POINT ( 'NONE',  ( 40.26954217208372455, -28.90384086642191619, 72.86986841596730358 ) ) ;
#21262 = CARTESIAN_POINT ( 'NONE',  ( 39.75915168707250302, 1.286317911113898260, 70.26145752964255564 ) ) ;
#21263 = CARTESIAN_POINT ( 'NONE',  ( 36.89935272106204422, -5.213682088886100630, 69.52238214136768590 ) ) ;
#21264 = EDGE_LOOP ( 'NONE', ( #5838, #8070, #2240, #15889 ) ) ;
#21265 = CARTESIAN_POINT ( 'NONE',  ( 43.81606138205700063, -36.10876147765401356, 70.30501292737011454 ) ) ;
#21266 = AXIS2_PLACEMENT_3D ( 'NONE', #15518, #11418, #19145 ) ;
#21267 = CARTESIAN_POINT ( 'NONE',  ( 39.31564783533279694, -7.303840866421912104, 70.72433947564853440 ) ) ;
#21268 = VECTOR ( 'NONE', #548, 1000.000000000000114 ) ;
#21269 = AXIS2_PLACEMENT_3D ( 'NONE', #13197, #19482, #1827 ) ;
#21270 = LINE ( 'NONE', #1930, #19648 ) ;
#21271 = EDGE_LOOP ( 'NONE', ( #20709, #3772, #21193, #22936, #13516, #10344, #12732, #12965, #21457, #10664, #5669, #21692, #3063 ) ) ;
#21272 = DIRECTION ( 'NONE',  ( -1.000000000000000000, -1.187136597504755470E-16, -8.249087426255172434E-17 ) ) ;
#21273 = CARTESIAN_POINT ( 'NONE',  ( 43.06606138205700063, 42.19123852234599070, 73.55501292736987295 ) ) ;
#21274 = CARTESIAN_POINT ( 'NONE',  ( 37.61123632939164452, -11.70384086642191335, 69.02690120949094421 ) ) ;
#21275 = CARTESIAN_POINT ( 'NONE',  ( 33.31606138205700773, -39.60075215179220720, 69.23691647014479145 ) ) ;
#21276 = CARTESIAN_POINT ( 'NONE',  ( 31.81606138205700418, 40.39281886181299797, 82.55501292736983032 ) ) ;
#21277 = CARTESIAN_POINT ( 'NONE',  ( 39.98359781491296161, -12.41368208888610525, 71.86517103874047052 ) ) ;
#21278 = PLANE ( 'NONE',  #23236 ) ;
#21279 = PLANE ( 'NONE',  #13460 ) ;
#21280 = ORIENTED_EDGE ( 'NONE', *, *, #1859, .F. ) ;
#21281 = DIRECTION ( 'NONE',  ( 2.453269466693404537E-16, -0.7071067811865489050, 0.7071067811865460184 ) ) ;
#21282 = CARTESIAN_POINT ( 'NONE',  ( 36.68196826583682935, -8.003840866421912281, 70.79240656858108593 ) ) ;
#21283 = PRODUCT_CONTEXT ( 'NONE', #15728, 'mechanical' ) ;
#21284 = EDGE_CURVE ( 'NONE', #11368, #21068, #24122, .T. ) ;
#21285 = CARTESIAN_POINT ( 'NONE',  ( 32.81106138205699807, 4.124002793203064066, 6.312068993173404863 ) ) ;
#21286 = CARTESIAN_POINT ( 'NONE',  ( 39.95015449827720744, -20.61368208888610454, 70.79240656858105751 ) ) ;
#21287 = EDGE_CURVE ( 'NONE', #2469, #15804, #3686, .T. ) ;
#21288 = AXIS2_PLACEMENT_3D ( 'NONE', #9203, #4937, #3245 ) ;
#21289 = FACE_OUTER_BOUND ( 'NONE', #15850, .T. ) ;
#21290 = CARTESIAN_POINT ( 'NONE',  ( 38.93415946300896024, -15.50384086642190873, 69.66206559358661821 ) ) ;
#21291 = CARTESIAN_POINT ( 'NONE',  ( 38.18531088334250967, -5.204193249396277032, 83.31006292736994112 ) ) ;
#21292 = CARTESIAN_POINT ( 'NONE',  ( 36.80608444377001121, -15.31368208888610383, 70.35351908239857721 ) ) ;
#21293 = VERTEX_POINT ( 'NONE', #9866 ) ;
#21294 = CARTESIAN_POINT ( 'NONE',  ( 39.64521430340304420, -20.81368208888610027, 69.45876917294175712 ) ) ;
#21295 = EDGE_LOOP ( 'NONE', ( #25401, #10979, #9227, #3903, #4380, #3288, #10629, #9527 ) ) ;
#21296 = CARTESIAN_POINT ( 'NONE',  ( 35.64099152588522657, 40.39281886181299797, 84.30501292736984453 ) ) ;
#21297 = CARTESIAN_POINT ( 'NONE',  ( 35.81606138205700063, 41.44123852234599781, 75.30501292736988717 ) ) ;
#21298 = CARTESIAN_POINT ( 'NONE',  ( 37.89291511884479036, -22.50384086642191050, 72.49843995877330372 ) ) ;
#21299 = ORIENTED_EDGE ( 'NONE', *, *, #18472, .F. ) ;
#21300 = ORIENTED_EDGE ( 'NONE', *, *, #348, .F. ) ;
#21301 = CARTESIAN_POINT ( 'NONE',  ( 40.31606138205700773, -11.22674583108233115, 81.40610939240433197 ) ) ;
#21302 = EDGE_CURVE ( 'NONE', #5640, #16406, #19774, .T. ) ;
#21303 = DIRECTION ( 'NONE',  ( 0.000000000000000000, 0.000000000000000000, 1.000000000000000000 ) ) ;
#21304 = ORIENTED_EDGE ( 'NONE', *, *, #4695, .T. ) ;
#21305 = SURFACE_STYLE_FILL_AREA ( #24770 ) ;
#21306 = CARTESIAN_POINT ( 'NONE',  ( 39.95015449827720744, -1.003840866421912281, 71.96809898377888715 ) ) ;
#21307 = VECTOR ( 'NONE', #18424, 1000.000000000000000 ) ;
#21308 = VECTOR ( 'NONE', #24110, 1000.000000000000000 ) ;
#21309 = AXIS2_PLACEMENT_3D ( 'NONE', #12840, #20691, #10904 ) ;
#21310 = FACE_OUTER_BOUND ( 'NONE', #23575, .T. ) ;
#21311 = FACE_OUTER_BOUND ( 'NONE', #1977, .T. ) ;
#21312 = ORIENTED_EDGE ( 'NONE', *, *, #8068, .T. ) ;
#21313 = ORIENTED_EDGE ( 'NONE', *, *, #11505, .F. ) ;
#21314 = FACE_OUTER_BOUND ( 'NONE', #24628, .T. ) ;
#21315 = DIRECTION ( 'NONE',  ( -1.000000000000000000, -1.734723475976804876E-16, 1.734723475976814737E-16 ) ) ;
#21316 = CARTESIAN_POINT ( 'NONE',  ( 38.82593461698264292, -28.70384086642190979, 73.13360434286902034 ) ) ;
#21317 = FACE_OUTER_BOUND ( 'NONE', #25229, .T. ) ;
#21318 = VERTEX_POINT ( 'NONE', #17724 ) ;
#21319 = CARTESIAN_POINT ( 'NONE',  ( 34.81606138205700773, -21.26162886970023536, 44.16441745890789150 ) ) ;
#21320 = LINE ( 'NONE', #1599, #18506 ) ;
#21321 = CARTESIAN_POINT ( 'NONE',  ( 43.31606138205700063, -12.76023008545320181, 21.53290024082827969 ) ) ;
#21322 = CARTESIAN_POINT ( 'NONE',  ( 37.21915885897815457, -4.203840866421909794, 71.67976084211552745 ) ) ;
#21323 = EDGE_LOOP ( 'NONE', ( #272, #8754, #24986, #9928 ) ) ;
#21324 = AXIS2_PLACEMENT_3D ( 'NONE', #21200, #17469, #5734 ) ;
#21325 = DIRECTION ( 'NONE',  ( 1.000000000000000000, 1.734723475976804876E-16, -1.734723475976814737E-16 ) ) ;
#21326 = ORIENTED_EDGE ( 'NONE', *, *, #23720, .F. ) ;
#21327 = ORIENTED_EDGE ( 'NONE', *, *, #18660, .T. ) ;
#21328 = CARTESIAN_POINT ( 'NONE',  ( 33.31606138205700773, -20.93319939328399926, 43.78741072286599945 ) ) ;
#21329 = CARTESIAN_POINT ( 'NONE',  ( 38.37017380507020192, -12.01368208888610134, 72.51602215082118619 ) ) ;
#21330 = CARTESIAN_POINT ( 'NONE',  ( 37.12184278917507640, -9.513682088886101340, 71.43714994484035685 ) ) ;
#21331 = EDGE_LOOP ( 'NONE', ( #11845, #7360, #24126, #7561 ) ) ;
#21332 = ORIENTED_EDGE ( 'NONE', *, *, #22010, .T. ) ;
#21333 = CARTESIAN_POINT ( 'NONE',  ( 39.48763425731081611, -21.82678658219787593, 29.70634659473178374 ) ) ;
#21334 = EDGE_CURVE ( 'NONE', #20889, #17789, #22209, .T. ) ;
#21335 = CARTESIAN_POINT ( 'NONE',  ( 46.81606138205697221, -3.542416608809818346, -4.744096181734387407 ) ) ;
#21336 = ORIENTED_EDGE ( 'NONE', *, *, #12903, .T. ) ;
#21337 = CARTESIAN_POINT ( 'NONE',  ( 33.40064408022072939, 41.90149715599300606, 79.37823623207322044 ) ) ;
#21338 = CARTESIAN_POINT ( 'NONE',  ( 36.64852494920107517, -14.20384086642191157, 71.86517103874048473 ) ) ;
#21339 =( GEOMETRIC_REPRESENTATION_CONTEXT ( 3 ) GLOBAL_UNCERTAINTY_ASSIGNED_CONTEXT ( ( #24129 ) ) GLOBAL_UNIT_ASSIGNED_CONTEXT ( ( #12385, #14428, #4639 ) ) REPRESENTATION_CONTEXT ( 'NONE', 'WORKASPACE' ) );
#21340 = DIRECTION ( 'NONE',  ( 1.734723475976804876E-16, 3.491481338843135327E-15, 1.000000000000000000 ) ) ;
#21341 = CARTESIAN_POINT ( 'NONE',  ( 39.37952058850012804, -18.61368208888609743, 70.97781676520601479 ) ) ;
#21342 = ORIENTED_EDGE ( 'NONE', *, *, #14464, .F. ) ;
#21343 = VECTOR ( 'NONE', #14101, 1000.000000000000000 ) ;
#21344 = CARTESIAN_POINT ( 'NONE',  ( 36.31606138205700063, -12.40281258615396176, 20.95421293576468358 ) ) ;
#21345 = LINE ( 'NONE', #23019, #697 ) ;
#21346 = CARTESIAN_POINT ( 'NONE',  ( 41.31606138205700063, 7.611641054560886133, 65.67022133066943468 ) ) ;
#21347 = EDGE_CURVE ( 'NONE', #19881, #4087, #6380, .T. ) ;
#21348 = EDGE_CURVE ( 'NONE', #7324, #7168, #55, .T. ) ;
#21349 = CARTESIAN_POINT ( 'NONE',  ( 40.05520938202761982, -6.207949209480774222, 83.25749895850351834 ) ) ;
#21350 = CYLINDRICAL_SURFACE ( 'NONE', #9403, 0.7500000000000006661 ) ;
#21351 = CIRCLE ( 'NONE', #4893, 2.500000000000002220 ) ;
#21352 = LINE ( 'NONE', #1887, #17683 ) ;
#21353 = ADVANCED_FACE ( 'NONE', ( #302 ), #23879, .T. ) ;
#21354 = ORIENTED_EDGE ( 'NONE', *, *, #12501, .T. ) ;
#21355 = CARTESIAN_POINT ( 'NONE',  ( 41.31606138205700063, -20.93319939328399926, 43.78741072286599945 ) ) ;
#21356 = ORIENTED_EDGE ( 'NONE', *, *, #12099, .T. ) ;
#21357 = VERTEX_POINT ( 'NONE', #19292 ) ;
#21358 = CARTESIAN_POINT ( 'NONE',  ( 36.29569395875881099, -8.303840866421920097, 72.77780686321129622 ) ) ;
#21359 = AXIS2_PLACEMENT_3D ( 'NONE', #16891, #15329, #20760 ) ;
#21360 = ADVANCED_FACE ( 'NONE', ( #2364 ), #20870, .T. ) ;
#21361 = DIRECTION ( 'NONE',  ( 0.000000000000000000, 0.6568589528324747517, -0.7540134720837718962 ) ) ;
#21362 = CARTESIAN_POINT ( 'NONE',  ( 37.33957961208646736, -13.81368208888610916, 72.81632618279321889 ) ) ;
#21363 = CIRCLE ( 'NONE', #10271, 1.000000000000000888 ) ;
#21364 = ORIENTED_EDGE ( 'NONE', *, *, #20449, .F. ) ;
#21365 = CARTESIAN_POINT ( 'NONE',  ( 46.81606138205704326, -28.78650366438485975, 68.66406800134920729 ) ) ;
#21366 = PLANE ( 'NONE',  #1401 ) ;
#21367 = CARTESIAN_POINT ( 'NONE',  ( 40.55423172469004811, -24.41368208888610880, 72.05058123536539938 ) ) ;
#21368 = EDGE_LOOP ( 'NONE', ( #21555, #21474, #10016, #2741 ) ) ;
#21369 = VECTOR ( 'NONE', #10909, 1000.000000000000000 ) ;
#21370 = DIRECTION ( 'NONE',  ( 0.000000000000000000, 0.8967398287344627850, 0.4425581086832401922 ) ) ;
#21371 = AXIS2_PLACEMENT_3D ( 'NONE', #17905, #227, #991 ) ;
#21372 = FACE_OUTER_BOUND ( 'NONE', #4879, .T. ) ;
#21373 = DIRECTION ( 'NONE',  ( 0.000000000000000000, -1.000000000000000000, 2.999999999999999839E-15 ) ) ;
#21374 = ADVANCED_FACE ( 'NONE', ( #23639 ), #15783, .T. ) ;
#21375 = SHAPE_REPRESENTATION_RELATIONSHIP ( 'NONE' , 'NONE' ,  #15514, #6771 ) ;
#21376 = AXIS2_PLACEMENT_3D ( 'NONE', #558, #10119, #22079 ) ;
#21377 = EDGE_CURVE ( 'NONE', #19911, #11722, #12310, .T. ) ;
#21378 = FACE_OUTER_BOUND ( 'NONE', #17980, .T. ) ;
#21379 = DIRECTION ( 'NONE',  ( 1.734723475976814737E-16, -1.000000000000000000, 3.491481338843135327E-15 ) ) ;
#21380 = EDGE_CURVE ( 'NONE', #11138, #16259, #21707, .T. ) ;
#21381 = VECTOR ( 'NONE', #11139, 1000.000000000000000 ) ;
#21382 = CARTESIAN_POINT ( 'NONE',  ( 38.37017380507018771, -9.603840866421911926, 70.24448340153877268 ) ) ;
#21383 = CARTESIAN_POINT ( 'NONE',  ( 38.37017380507020192, -28.01368208888610312, 72.51602215082114355 ) ) ;
#21384 = EDGE_CURVE ( 'NONE', #7327, #23347, #3985, .T. ) ;
#21385 = EDGE_LOOP ( 'NONE', ( #21176, #15121, #10071, #12465 ) ) ;
#21386 = AXIS2_PLACEMENT_3D ( 'NONE', #13950, #22054, #6095 ) ;
#21387 = DIRECTION ( 'NONE',  ( -1.225631768639319301E-15, 0.4425581086832399147, -0.8967398287344627850 ) ) ;
#21388 = DIRECTION ( 'NONE',  ( 0.000000000000000000, 0.4425581086832399702, -0.8967398287344626739 ) ) ;
#21389 = ORIENTED_EDGE ( 'NONE', *, *, #20187, .F. ) ;
#21390 = VERTEX_POINT ( 'NONE', #11934 ) ;
#21391 = AXIS2_PLACEMENT_3D ( 'NONE', #17853, #21831, #2110 ) ;
#21392 = CARTESIAN_POINT ( 'NONE',  ( 36.68196826583682935, -2.003840866421909617, 70.79240656858108593 ) ) ;
#21393 = EDGE_CURVE ( 'NONE', #16850, #14470, #2113, .T. ) ;
#21394 = CARTESIAN_POINT ( 'NONE',  ( 40.14115730948191185, -0.5136820888861047818, 71.32335560751961623 ) ) ;
#21395 = CARTESIAN_POINT ( 'NONE',  ( 40.77203464402485622, -0.5136820888861047818, 71.32335560751961623 ) ) ;
#21396 = VERTEX_POINT ( 'NONE', #20026 ) ;
#21397 = DIRECTION ( 'NONE',  ( 0.000000000000000000, -3.965082230804126670E-15, -1.000000000000000000 ) ) ;
#21398 = CARTESIAN_POINT ( 'NONE',  ( 37.60469502381300799, -6.403840866421910860, 72.26730301774236409 ) ) ;
#21399 = DIRECTION ( 'NONE',  ( -1.734723475976805122E-16, -3.491481338843134933E-15, -1.000000000000000000 ) ) ;
#21400 = ORIENTED_EDGE ( 'NONE', *, *, #8626, .T. ) ;
#21401 = CARTESIAN_POINT ( 'NONE',  ( 37.31606138205700063, 42.19123852234599781, 74.30501292736987295 ) ) ;
#21402 = FACE_OUTER_BOUND ( 'NONE', #2640, .T. ) ;
#21403 = CARTESIAN_POINT ( 'NONE',  ( 35.86008812008917346, -12.10384086642191548, 71.32335560751961623 ) ) ;
#21404 = CARTESIAN_POINT ( 'NONE',  ( 43.81606138205700063, 44.92314894770294131, 81.37823623207322044 ) ) ;
#21405 = CARTESIAN_POINT ( 'NONE',  ( 33.31606138205700773, -16.48551471403133206, 77.11349248448009064 ) ) ;
#21406 = CARTESIAN_POINT ( 'NONE',  ( 36.49096545463212493, -13.51368208888610489, 71.43714994484034264 ) ) ;
#21407 = DIRECTION ( 'NONE',  ( -9.925461516413211857E-16, 0.8967398287344600094, 0.4425581086832455213 ) ) ;
#21408 = EDGE_CURVE ( 'NONE', #12627, #9628, #12187, .T. ) ;
#21409 = DIRECTION ( 'NONE',  ( -8.381647117973248681E-31, -0.7071067811865460184, -0.7071067811865489050 ) ) ;
#21410 = AXIS2_PLACEMENT_3D ( 'NONE', #24941, #3065, #20597 ) ;
#21411 = VERTEX_POINT ( 'NONE', #23757 ) ;
#21412 = CARTESIAN_POINT ( 'NONE',  ( 38.31606138205700063, -4.070846987468769385, 59.14016975459033887 ) ) ;
#21413 = CARTESIAN_POINT ( 'NONE',  ( 36.64852494920107517, -0.2038408664219101829, 71.86517103874049894 ) ) ;
#21414 = APPLICATION_PROTOCOL_DEFINITION ( 'draft international standard', 'automotive_design', 1998, #4370 ) ;
#21415 = CARTESIAN_POINT ( 'NONE',  ( 44.06606138205700063, 40.92314894770294842, 83.08534301325974525 ) ) ;
#21416 = CARTESIAN_POINT ( 'NONE',  ( 38.82593461698262871, -16.91368208888610170, 69.62690120949091011 ) ) ;
#21417 = DIRECTION ( 'NONE',  ( 1.000000000000000000, 0.000000000000000000, 0.000000000000000000 ) ) ;
#21418 = CARTESIAN_POINT ( 'NONE',  ( 38.37017380507018771, -19.60384086642191193, 69.64448340153877837 ) ) ;
#21419 = DIRECTION ( 'NONE',  ( 1.734723475976814737E-16, -1.000000000000000000, 3.491481338843135327E-15 ) ) ;
#21420 = VECTOR ( 'NONE', #22351, 1000.000000000000000 ) ;
#21421 = CARTESIAN_POINT ( 'NONE',  ( 37.80618814713140097, -17.91368208888609814, 73.13360434286903455 ) ) ;
#21422 = ORIENTED_EDGE ( 'NONE', *, *, #15856, .T. ) ;
#21423 = CARTESIAN_POINT ( 'NONE',  ( 40.26954217208371034, -22.71368208888610241, 69.89063713639258424 ) ) ;
#21424 = EDGE_LOOP ( 'NONE', ( #22482, #3139, #16701, #9201 ) ) ;
#21425 = CARTESIAN_POINT ( 'NONE',  ( 43.30090830489194786, -32.87633672316712108, 59.29685926994373091 ) ) ;
#21426 = CARTESIAN_POINT ( 'NONE',  ( 44.81606138205700063, 41.44123852234599781, 74.30501292736987295 ) ) ;
#21427 = AXIS2_PLACEMENT_3D ( 'NONE', #16192, #16958, #12723 ) ;
#21428 = CARTESIAN_POINT ( 'NONE',  ( 39.24876120206129571, -24.90384086642191264, 72.12822762946746025 ) ) ;
#21429 = VERTEX_POINT ( 'NONE', #21834 ) ;
#21430 = EDGE_LOOP ( 'NONE', ( #3753, #25166, #9266, #19125, #24225, #16070 ) ) ;
#21431 = CARTESIAN_POINT ( 'NONE',  ( 1.291443647867872416E-14, -30.45978664257872381, 43.58374455696571914 ) ) ;
#21432 = DIRECTION ( 'NONE',  ( 0.000000000000000000, -2.999999999999999839E-15, -1.000000000000000000 ) ) ;
#21433 = VERTEX_POINT ( 'NONE', #10367 ) ;
#21434 = CARTESIAN_POINT ( 'NONE',  ( 39.02088643472237806, -28.70384086642191690, 73.73360434286898624 ) ) ;
#21435 = EDGE_CURVE ( 'NONE', #24927, #821, #2492, .T. ) ;
#21436 = EDGE_CURVE ( 'NONE', #9471, #24226, #24624, .T. ) ;
#21437 = DIRECTION ( 'NONE',  ( 0.000000000000000000, 0.8191520442889929088, 0.5735764363510444941 ) ) ;
#21438 = CARTESIAN_POINT ( 'NONE',  ( 39.02088643472237095, -4.913682088886102584, 69.02690120949094421 ) ) ;
#21439 = PRODUCT_RELATED_PRODUCT_CATEGORY ( 'part', '', ( #7876 ) ) ;
#21440 = LINE ( 'NONE', #11667, #6507 ) ;
#21441 = ORIENTED_EDGE ( 'NONE', *, *, #20519, .T. ) ;
#21442 = ORIENTED_EDGE ( 'NONE', *, *, #20949, .F. ) ;
#21443 = CARTESIAN_POINT ( 'NONE',  ( 38.31606138205702194, 1.691238522345987150, 73.11602215082119471 ) ) ;
#21444 = PLANE ( 'NONE',  #11408 ) ;
#21445 = CARTESIAN_POINT ( 'NONE',  ( 39.75915168707251723, -22.90384086642191264, 72.49904802271738902 ) ) ;
#21446 = SHAPE_REPRESENTATION_RELATIONSHIP ( 'NONE' , 'NONE' ,  #14587, #24269 ) ;
#21447 = DIRECTION ( 'NONE',  ( 0.000000000000000000, 1.000000000000000000, -6.938893903907222067E-15 ) ) ;
#21448 = AXIS2_PLACEMENT_3D ( 'NONE', #447, #11949, #14124 ) ;
#21449 = ORIENTED_EDGE ( 'NONE', *, *, #20649, .T. ) ;
#21450 = PLANE ( 'NONE',  #21324 ) ;
#21451 = EDGE_CURVE ( 'NONE', #3268, #19523, #22716, .T. ) ;
#21452 = CARTESIAN_POINT ( 'NONE',  ( 29.71606138205696368, 0.8576245772853353655, -1.570935883000529332 ) ) ;
#21453 = DIRECTION ( 'NONE',  ( -1.000000000000000000, -2.999999999999999839E-15, 0.000000000000000000 ) ) ;
#21454 = CARTESIAN_POINT ( 'NONE',  ( 37.38336156205273397, -3.903840866421911748, 70.63227792289248441 ) ) ;
#21455 = ORIENTED_EDGE ( 'NONE', *, *, #13023, .F. ) ;
#21456 = DIRECTION ( 'NONE',  ( 0.000000000000000000, 0.000000000000000000, 1.000000000000000000 ) ) ;
#21457 = ORIENTED_EDGE ( 'NONE', *, *, #8071, .T. ) ;
#21458 = ORIENTED_EDGE ( 'NONE', *, *, #22708, .T. ) ;
#21459 = PLANE ( 'NONE',  #13480 ) ;
#21460 = CARTESIAN_POINT ( 'NONE',  ( 37.69225076346193504, -9.813682088886100274, 72.33091598616827866 ) ) ;
#21461 = CARTESIAN_POINT ( 'NONE',  ( 37.60469502381300089, -13.21368208888610241, 70.49320253461759478 ) ) ;
#21462 = EDGE_LOOP ( 'NONE', ( #24146, #13927, #10129, #19360 ) ) ;
#21463 = ORIENTED_EDGE ( 'NONE', *, *, #20204, .F. ) ;
#21464 = CARTESIAN_POINT ( 'NONE',  ( 40.31606138205700773, -21.45740613484709769, 28.95788407061096237 ) ) ;
#21465 = LINE ( 'NONE', #21721, #13691 ) ;
#21466 = EDGE_LOOP ( 'NONE', ( #4967, #15049, #24885, #12921 ) ) ;
#21467 = LINE ( 'NONE', #20966, #12013 ) ;
#21468 = CARTESIAN_POINT ( 'NONE',  ( 39.98359781491296161, -19.20384086642191335, 70.89533451361945993 ) ) ;
#21469 = ADVANCED_FACE ( 'NONE', ( #4945 ), #7005, .T. ) ;
#21470 = EDGE_CURVE ( 'NONE', #7305, #13947, #14481, .T. ) ;
#21471 = FACE_OUTER_BOUND ( 'NONE', #20193, .T. ) ;
#21472 = AXIS2_PLACEMENT_3D ( 'NONE', #18211, #17166, #21032 ) ;
#21473 = CARTESIAN_POINT ( 'NONE',  ( 37.21915885897815457, -17.41368208888610170, 71.08074471024443142 ) ) ;
#21474 = ORIENTED_EDGE ( 'NONE', *, *, #17904, .F. ) ;
#21475 = ORIENTED_EDGE ( 'NONE', *, *, #14939, .F. ) ;
#21476 = FACE_OUTER_BOUND ( 'NONE', #18103, .T. ) ;
#21477 = CARTESIAN_POINT ( 'NONE',  ( 36.64852494920107517, -11.41368208888610525, 70.89533451361947414 ) ) ;
#21478 = LINE ( 'NONE', #23143, #21695 ) ;
#21479 = DIRECTION ( 'NONE',  ( 1.000000000000000000, -0.000000000000000000, 0.000000000000000000 ) ) ;
#21480 = CARTESIAN_POINT ( 'NONE',  ( 38.83610899671118943, -5.268519173439224268, 83.30989761756769951 ) ) ;
#21481 = DIRECTION ( 'NONE',  ( 1.000000000000000000, 0.000000000000000000, -0.000000000000000000 ) ) ;
#21482 = EDGE_CURVE ( 'NONE', #4612, #24795, #25184, .T. ) ;
#21483 = VECTOR ( 'NONE', #19280, 1000.000000000000114 ) ;
#21484 = AXIS2_PLACEMENT_3D ( 'NONE', #19947, #2282, #23286 ) ;
#21485 = DIRECTION ( 'NONE',  ( -6.505213034913079606E-17, 1.000000000000000000, -3.491481338843135327E-15 ) ) ;
#21486 =( REPRESENTATION_RELATIONSHIP ('NONE','NONE', #17377, #7525 ) REPRESENTATION_RELATIONSHIP_WITH_TRANSFORMATION ( #3893 )SHAPE_REPRESENTATION_RELATIONSHIP( ) );
#21487 = ORIENTED_EDGE ( 'NONE', *, *, #14604, .T. ) ;
#21488 = TOROIDAL_SURFACE ( 'NONE', #14075, 1.000000000000000000, 1.000000000000000000 ) ;
#21489 = DIRECTION ( 'NONE',  ( 1.000000000000000000, 1.000000000000000078E-15, 0.000000000000000000 ) ) ;
#21490 = VERTEX_POINT ( 'NONE', #10625 ) ;
#21491 = VERTEX_POINT ( 'NONE', #18476 ) ;
#21492 = CARTESIAN_POINT ( 'NONE',  ( 35.86008812008917346, -10.10384086642191548, 71.32335560751961623 ) ) ;
#21493 = ORIENTED_EDGE ( 'NONE', *, *, #15467, .T. ) ;
#21494 = CARTESIAN_POINT ( 'NONE',  ( 42.96606138205697789, -6.230354416574639842, -1.331254207427787328 ) ) ;
#21495 = CARTESIAN_POINT ( 'NONE',  ( 38.93415946300897446, -14.11368208888610631, 73.09843995877329803 ) ) ;
#21496 = ORIENTED_EDGE ( 'NONE', *, *, #458, .T. ) ;
#21497 = PLANE ( 'NONE',  #14206 ) ;
#21498 = LINE ( 'NONE', #17381, #9245 ) ;
#21499 = CARTESIAN_POINT ( 'NONE',  ( 40.26954217208371034, -18.71368208888610241, 69.89063713639258424 ) ) ;
#21500 = ORIENTED_EDGE ( 'NONE', *, *, #18785, .T. ) ;
#21501 = CIRCLE ( 'NONE', #8345, 1.549999999999995826 ) ;
#21502 = CARTESIAN_POINT ( 'NONE',  ( 41.81606138205700063, -2.300394311618905174, 46.75701924734788406 ) ) ;
#21503 = CARTESIAN_POINT ( 'NONE',  ( 45.81606138205700063, 36.92314894770294131, 80.37823623207323465 ) ) ;
#21504 = AXIS2_PLACEMENT_3D ( 'NONE', #20837, #21214, #13368 ) ;
#21505 = DIRECTION ( 'NONE',  ( 1.000000000000000000, 0.000000000000000000, 0.000000000000000000 ) ) ;
#21506 = CARTESIAN_POINT ( 'NONE',  ( 30.81606138205700773, 40.39281886181299797, 81.44836866983821722 ) ) ;
#21507 = VECTOR ( 'NONE', #15063, 1000.000000000000227 ) ;
#21508 = EDGE_CURVE ( 'NONE', #170, #13976, #20796, .T. ) ;
#21509 = AXIS2_PLACEMENT_3D ( 'NONE', #17902, #347, #23800 ) ;
#21510 = CARTESIAN_POINT ( 'NONE',  ( 43.06606138205700063, -34.55876147765400219, 75.30501292737011454 ) ) ;
#21511 = CARTESIAN_POINT ( 'NONE',  ( 37.89291511884479036, -14.50384086642191228, 72.49843995877330372 ) ) ;
#21512 = CARTESIAN_POINT ( 'NONE',  ( 36.80608444377001121, -1.313682088886099386, 70.35351908239860563 ) ) ;
#21513 = ORIENTED_EDGE ( 'NONE', *, *, #2938, .T. ) ;
#21514 = DIRECTION ( 'NONE',  ( 0.000000000000000000, 4.476705744456288765E-15, 1.000000000000000000 ) ) ;
#21515 = VECTOR ( 'NONE', #19745, 1000.000000000000000 ) ;
#21516 = DIRECTION ( 'NONE',  ( -0.1733269559585470521, -3.077057697073492856E-15, -0.9848643390529193686 ) ) ;
#21517 = EDGE_LOOP ( 'NONE', ( #5212, #9103, #17670, #3546, #14699 ) ) ;
#21518 = ORIENTED_EDGE ( 'NONE', *, *, #17382, .T. ) ;
#21519 = VECTOR ( 'NONE', #12841, 1000.000000000000000 ) ;
#21520 = CARTESIAN_POINT ( 'NONE',  ( 39.73277004305197124, -29.40384086642191264, 69.52238214136765748 ) ) ;
#21521 = VECTOR ( 'NONE', #1579, 1000.000000000000227 ) ;
#21522 = CARTESIAN_POINT ( 'NONE',  ( 37.21915885897815457, -23.41368208888610170, 71.08074471024441721 ) ) ;
#21523 = CARTESIAN_POINT ( 'NONE',  ( 35.86008812008917346, -5.513682088886105781, 71.43714994484035685 ) ) ;
#21524 = VERTEX_POINT ( 'NONE', #7137 ) ;
#21525 = PLANE ( 'NONE',  #1635 ) ;
#21526 = CARTESIAN_POINT ( 'NONE',  ( 39.51027997493896748, -5.103840866421911926, 71.43714994484034264 ) ) ;
#21527 = EDGE_CURVE ( 'NONE', #11368, #6775, #3130, .T. ) ;
#21528 = LINE ( 'NONE', #7365, #5653 ) ;
#21529 = EDGE_CURVE ( 'NONE', #1296, #10963, #5639, .T. ) ;
#21530 = ORIENTED_EDGE ( 'NONE', *, *, #20314, .T. ) ;
#21531 = VECTOR ( 'NONE', #5382, 1000.000000000000000 ) ;
#21532 = FACE_OUTER_BOUND ( 'NONE', #8183, .T. ) ;
#21533 = FACE_OUTER_BOUND ( 'NONE', #1478, .T. ) ;
#21534 = CARTESIAN_POINT ( 'NONE',  ( 36.36258059203030513, -11.90384086642191441, 69.89063713639259845 ) ) ;
#21535 = ADVANCED_FACE ( 'NONE', ( #2620 ), #9522, .T. ) ;
#21536 = EDGE_CURVE ( 'NONE', #14213, #17064, #23338, .T. ) ;
#21537 = ADVANCED_FACE ( 'NONE', ( #11645 ), #23215, .F. ) ;
#21538 = CARTESIAN_POINT ( 'NONE',  ( 43.31606138205700063, -27.60498114914042134, 57.04949906928993641 ) ) ;
#21539 = CARTESIAN_POINT ( 'NONE',  ( 37.14448850680319225, -22.27515649656511698, 29.48506754039016897 ) ) ;
#21540 = CARTESIAN_POINT ( 'NONE',  ( 39.29254315202756231, -16.81368208888610383, 69.94417936956672577 ) ) ;
#21541 = DIRECTION ( 'NONE',  ( 1.000000000000000000, 0.000000000000000000, 0.000000000000000000 ) ) ;
#21542 = DIRECTION ( 'NONE',  ( -0.1733269559585477460, -5.551115123125804790E-15, -0.9848643390529193686 ) ) ;
#21543 = CIRCLE ( 'NONE', #24811, 1.750000000000001554 ) ;
#21544 = DIRECTION ( 'NONE',  ( 0.000000000000000000, -1.000000000000000000, 2.999999999999999839E-15 ) ) ;
#21545 = VECTOR ( 'NONE', #23069, 1000.000000000000000 ) ;
#21546 = CARTESIAN_POINT ( 'NONE',  ( 36.87297107704151244, 0.09615913357809147133, 70.26145752964255564 ) ) ;
#21547 = ADVANCED_FACE ( 'NONE', ( #25389 ), #5582, .F. ) ;
#21548 = CARTESIAN_POINT ( 'NONE',  ( 43.23188216675521289, 3.685658823189455369, 6.335155785894674096 ) ) ;
#21549 = CARTESIAN_POINT ( 'NONE',  ( 37.33957961208646736, -19.81368208888611093, 72.81632618279321889 ) ) ;
#21550 = CARTESIAN_POINT ( 'NONE',  ( 45.06606138205707879, -39.99575152356565155, 63.13209164280871022 ) ) ;
#21551 = CIRCLE ( 'NONE', #25219, 1.500000000000001332 ) ;
#21552 = CARTESIAN_POINT ( 'NONE',  ( 37.33957961208645315, -19.80384086642191122, 69.94417936956672577 ) ) ;
#21553 = FACE_OUTER_BOUND ( 'NONE', #16002, .T. ) ;
#21554 = CARTESIAN_POINT ( 'NONE',  ( 36.87297107704152666, -11.71368208888611129, 72.49904802271740323 ) ) ;
#21555 = ORIENTED_EDGE ( 'NONE', *, *, #11638, .F. ) ;
#21556 = CARTESIAN_POINT ( 'NONE',  ( 38.26194895904383486, -23.01368208888610312, 69.04448340153878405 ) ) ;
#21557 = ORIENTED_EDGE ( 'NONE', *, *, #22175, .F. ) ;
#21558 = CARTESIAN_POINT ( 'NONE',  ( 44.71606138205694947, 3.586515973360805187, -0.5067327973472466329 ) ) ;
#21559 = AXIS2_PLACEMENT_3D ( 'NONE', #20238, #9042, #12779 ) ;
#21560 = CARTESIAN_POINT ( 'NONE',  ( 34.81606138205696510, -1.975699482566735776, -4.057200616784870206 ) ) ;
#21561 = CARTESIAN_POINT ( 'NONE',  ( 37.60469502381300799, -22.40384086642191264, 72.26730301774234988 ) ) ;
#21562 = ORIENTED_EDGE ( 'NONE', *, *, #6867, .F. ) ;
#21563 = EDGE_LOOP ( 'NONE', ( #3570, #6124 ) ) ;
#21564 = CARTESIAN_POINT ( 'NONE',  ( 35.31606138205700773, 7.282926244446937147, 65.60596383066929604 ) ) ;
#21565 = AXIS2_PLACEMENT_3D ( 'NONE', #11593, #19563, #11213 ) ;
#21566 = DIRECTION ( 'NONE',  ( -2.122643018205887308E-17, 1.000000000000000000, -3.120611096041553009E-15 ) ) ;
#21567 = DIRECTION ( 'NONE',  ( 0.000000000000000000, 1.000000000000000000, 0.000000000000000000 ) ) ;
#21568 = CARTESIAN_POINT ( 'NONE',  ( 39.29254315202757653, -0.8038408664219134359, 72.81632618279323310 ) ) ;
#21569 = CARTESIAN_POINT ( 'NONE',  ( 32.81606138205700773, 35.95440708241085304, 61.30501292736990138 ) ) ;
#21570 = CARTESIAN_POINT ( 'NONE',  ( 36.89935272106204422, -1.213682088886100630, 69.52238214136768590 ) ) ;
#21571 = CARTESIAN_POINT ( 'NONE',  ( 43.23147868389327897, 40.95934826813394380, 79.52109337493037344 ) ) ;
#21572 = ORIENTED_EDGE ( 'NONE', *, *, #812, .F. ) ;
#21573 = ORIENTED_EDGE ( 'NONE', *, *, #7580, .F. ) ;
#21574 = DIRECTION ( 'NONE',  ( -1.000000000000000000, 0.000000000000000000, 0.000000000000000000 ) ) ;
#21575 = STYLED_ITEM ( 'NONE', ( #7929 ), #21819 ) ;
#21576 = CARTESIAN_POINT ( 'NONE',  ( 33.31606138205700773, 7.611641054560886133, 65.67022133066943468 ) ) ;
#21577 = CARTESIAN_POINT ( 'NONE',  ( 37.25202387243754032, -20.40384086642191619, 72.75271321436731853 ) ) ;
#21578 = AXIS2_PLACEMENT_3D ( 'NONE', #18867, #7270, #6885 ) ;
#21579 =( LENGTH_UNIT ( ) NAMED_UNIT ( * ) SI_UNIT ( .MILLI., .METRE. ) );
#21580 = DIRECTION ( 'NONE',  ( -1.000000000000000000, -6.938893903907188146E-15, 8.673617379884188314E-16 ) ) ;
#21581 = ORIENTED_EDGE ( 'NONE', *, *, #18535, .T. ) ;
#21582 = CARTESIAN_POINT ( 'NONE',  ( 35.81606138205700063, -31.05876147765399864, 74.30501292737010033 ) ) ;
#21583 = CIRCLE ( 'NONE', #5133, 0.9999999999999937828 ) ;
#21584 = DIRECTION ( 'NONE',  ( -1.000000000000000000, 5.352861011585579840E-16, -1.605858303475673768E-30 ) ) ;
#21585 = CARTESIAN_POINT ( 'NONE',  ( 43.24580177837434292, 3.721690752961227755, 6.335617458560805382 ) ) ;
#21586 = CARTESIAN_POINT ( 'NONE',  ( 38.73920764526923932, -7.503840866421911393, 70.26206559358664094 ) ) ;
#21587 = ORIENTED_EDGE ( 'NONE', *, *, #4765, .F. ) ;
#21588 = EDGE_CURVE ( 'NONE', #20176, #22023, #17181, .T. ) ;
#21589 = CARTESIAN_POINT ( 'NONE',  ( 33.31606138205700773, 7.864187680719676443, 65.89022736311019912 ) ) ;
#21590 = ORIENTED_EDGE ( 'NONE', *, *, #16006, .T. ) ;
#21591 = EDGE_CURVE ( 'NONE', #20374, #20593, #7516, .T. ) ;
#21592 = ORIENTED_EDGE ( 'NONE', *, *, #10045, .F. ) ;
#21593 = CARTESIAN_POINT ( 'NONE',  ( 45.06606138205697221, -5.022037326221688858, -5.474317061061731771 ) ) ;
#21594 = CARTESIAN_POINT ( 'NONE',  ( 39.51027997493896748, -12.51368208888610134, 71.32335560751960202 ) ) ;
#21595 = CARTESIAN_POINT ( 'NONE',  ( 38.00113996487114321, -9.913682088886099919, 72.53360434286905445 ) ) ;
#21596 = EDGE_LOOP ( 'NONE', ( #21708, #16309, #22880, #22600 ) ) ;
#21597 = EDGE_LOOP ( 'NONE', ( #21587, #11215, #15911, #400 ) ) ;
#21598 = DIRECTION ( 'NONE',  ( 0.000000000000000000, 9.938893903907240838E-15, 1.000000000000000000 ) ) ;
#21599 = PLANE ( 'NONE',  #6676 ) ;
#21600 = ORIENTED_EDGE ( 'NONE', *, *, #16028, .T. ) ;
#21601 = DIRECTION ( 'NONE',  ( 1.000000000000000000, -5.510910596163088391E-31, -1.836970198721029688E-16 ) ) ;
#21602 = CARTESIAN_POINT ( 'NONE',  ( 36.87297107704149823, -15.90384086642190908, 70.26145752964252722 ) ) ;
#21603 = AXIS2_PLACEMENT_3D ( 'NONE', #9063, #24736, #24477 ) ;
#21604 = CARTESIAN_POINT ( 'NONE',  ( 36.31606138205700063, -20.44477830400171570, 75.97174273075597739 ) ) ;
#21605 = CARTESIAN_POINT ( 'NONE',  ( 35.81606138205700063, 37.44123852234599781, 74.30501292736988717 ) ) ;
#21606 = CARTESIAN_POINT ( 'NONE',  ( 38.26194895904383486, -19.01368208888609956, 70.24448340153875847 ) ) ;
#21607 = ORIENTED_EDGE ( 'NONE', *, *, #18387, .F. ) ;
#21608 = VERTEX_POINT ( 'NONE', #19738 ) ;
#21609 = CARTESIAN_POINT ( 'NONE',  ( 38.96303889229209716, -5.307214332739725648, 83.30462760643098363 ) ) ;
#21610 = CARTESIAN_POINT ( 'NONE',  ( 39.75915168707250302, -12.71368208888610063, 70.26145752964252722 ) ) ;
#21611 = LINE ( 'NONE', #7830, #2375 ) ;
#21612 = CARTESIAN_POINT ( 'NONE',  ( 34.06606138205700773, 2.740850673309605412, 6.112030963703427133 ) ) ;
#21613 = FACE_OUTER_BOUND ( 'NONE', #25141, .T. ) ;
#21614 = CARTESIAN_POINT ( 'NONE',  ( 40.15363366728724515, -29.10876147765395672, 71.30696959218165887 ) ) ;
#21615 = ADVANCED_FACE ( 'NONE', ( #21553 ), #8277, .T. ) ;
#21616 = DIRECTION ( 'NONE',  ( 1.000000000000000000, 0.000000000000000000, 0.000000000000000000 ) ) ;
#21617 = ADVANCED_FACE ( 'NONE', ( #5834 ), #21672, .T. ) ;
#21618 = ORIENTED_EDGE ( 'NONE', *, *, #9585, .F. ) ;
#21619 = CARTESIAN_POINT ( 'NONE',  ( 29.81606138205705037, -30.46100403034036219, 72.05704881431053366 ) ) ;
#21620 = ORIENTED_EDGE ( 'NONE', *, *, #22789, .T. ) ;
#21621 = ORIENTED_EDGE ( 'NONE', *, *, #13097, .T. ) ;
#21622 = CARTESIAN_POINT ( 'NONE',  ( 40.77203464402485622, -7.103840866421913702, 71.43714994484034264 ) ) ;
#21623 = ORIENTED_EDGE ( 'NONE', *, *, #20581, .T. ) ;
#21624 = DIRECTION ( 'NONE',  ( 0.000000000000000000, -1.000000000000000000, 2.999999999999999839E-15 ) ) ;
#21625 = CARTESIAN_POINT ( 'NONE',  ( 36.68196826583682935, -17.61368208888610454, 71.96809898377888715 ) ) ;
#21626 = ORIENTED_EDGE ( 'NONE', *, *, #5219, .F. ) ;
#21627 = DIRECTION ( 'NONE',  ( -1.000000000000000000, -3.091505625455828697E-15, -4.515976121274772923E-17 ) ) ;
#21628 = PLANE ( 'NONE',  #12532 ) ;
#21629 = EDGE_CURVE ( 'NONE', #5237, #21411, #10167, .T. ) ;
#21630 = CARTESIAN_POINT ( 'NONE',  ( 37.61123632939165873, -11.91368208888610880, 73.73360434286898624 ) ) ;
#21631 = ORIENTED_EDGE ( 'NONE', *, *, #3030, .F. ) ;
#21632 = DIRECTION ( 'NONE',  ( -1.000000000000000000, 0.000000000000000000, 0.000000000000000000 ) ) ;
#21633 = LINE ( 'NONE', #7125, #549 ) ;
#21634 = DIRECTION ( 'NONE',  ( -1.000000000000000000, -2.999999999999999839E-15, 0.000000000000000000 ) ) ;
#21635 = CARTESIAN_POINT ( 'NONE',  ( 44.71606138205696368, -0.07962245140794195486, -2.393377716359348817 ) ) ;
#21636 = CARTESIAN_POINT ( 'NONE',  ( 38.00113996487112189, -15.70384086642191157, 70.22690120949090442 ) ) ;
#21637 = CARTESIAN_POINT ( 'NONE',  ( 39.82603832034400426, -2.313682088886107380, 72.40698646996135324 ) ) ;
#21638 = VERTEX_POINT ( 'NONE', #5965 ) ;
#21639 = CARTESIAN_POINT ( 'NONE',  ( 32.31606138205700063, -20.88462213365835041, 44.49284693532412405 ) ) ;
#21640 = DIRECTION ( 'NONE',  ( 0.000000000000000000, 1.000000000000000000, 0.000000000000000000 ) ) ;
#21641 = VERTEX_POINT ( 'NONE', #15993 ) ;
#21642 = ORIENTED_EDGE ( 'NONE', *, *, #22369, .T. ) ;
#21643 = CARTESIAN_POINT ( 'NONE',  ( 38.37017380507018771, -27.60384086642191548, 69.04448340153878405 ) ) ;
#21644 = VECTOR ( 'NONE', #8905, 1000.000000000000000 ) ;
#21645 = CARTESIAN_POINT ( 'NONE',  ( 39.31564783533280405, -26.31368208888610027, 72.03616607671136762 ) ) ;
#21646 = B_SPLINE_SURFACE_WITH_KNOTS ( 'NONE', 1, 3, ( 
 ( #450, #7955, #17999, #321, #16171, #16649, #13748, #8201, #2129, #24024, #10011, #2848, #200, #16048, #18581, #15919, #919, #11824 ),
 ( #8811, #21604, #19662, #2003, #20780, #11372, #14840, #9067, #24990, #8928, #7375, #12799, #13305, #15219, #20901, #3236, #11250, #18716 ),
 ( #13048, #23072, #17041, #11116, #18835, #3372, #13178, #19215, #5313, #3114, #22697, #19100, #24869, #1438, #5437, #9321, #24740, #5056 ),
 ( #7246, #20642, #1174, #10984, #21031, #18970, #16911, #21157, #7117, #1551, #15094, #22951, #9442, #14972, #22829, #17165, #5190, #3498 ) ),
 .UNSPECIFIED., .F., .F., .F.,
 ( 2, 1, 1, 2 ),
 ( 4, 2, 2, 2, 2, 2, 2, 2, 4 ),
 ( -0.01000000000000000021, 0.000000000000000000, 1.000000000000000000, 1.010099999999999998 ),
 ( 0.000000000000000000, 0.0003925198642609844754, 0.0007850397285219689507, 0.001177559592782951962, 0.001570079457043939853, 0.001962599321304919937, 0.002355119185565904792, 0.002747639049826890081, 0.003140158914087874936 ),
 .UNSPECIFIED. ) ;
#21647 = CARTESIAN_POINT ( 'NONE',  ( 39.02088643472237095, -0.9136820888861024725, 69.02690120949094421 ) ) ;
#21648 = ORIENTED_EDGE ( 'NONE', *, *, #23324, .F. ) ;
#21649 = DIRECTION ( 'NONE',  ( 0.000000000000000000, 1.000000000000000000, -2.999999999999999839E-15 ) ) ;
#21650 = CARTESIAN_POINT ( 'NONE',  ( 38.73920764526923932, 0.4961591335780889955, 70.26206559358665515 ) ) ;
#21651 = DIRECTION ( 'NONE',  ( -1.000000000000000000, 0.000000000000000000, 0.000000000000000000 ) ) ;
#21652 = ORIENTED_EDGE ( 'NONE', *, *, #721, .T. ) ;
#21653 = CARTESIAN_POINT ( 'NONE',  ( 29.81606138205707168, -37.70325315460882365, 65.37863370302704880 ) ) ;
#21654 = LINE ( 'NONE', #19097, #6739 ) ;
#21655 = EDGE_CURVE ( 'NONE', #536, #19510, #20046, .T. ) ;
#21656 = CARTESIAN_POINT ( 'NONE',  ( 36.98690846071097127, -3.803840866421912992, 69.45876917294177133 ) ) ;
#21657 = CARTESIAN_POINT ( 'NONE',  ( 32.81606138205700773, 18.19123852234599426, 73.05501292736995822 ) ) ;
#21658 = CARTESIAN_POINT ( 'NONE',  ( 46.81606138205701484, -19.24645833192446176, 25.04281637636312041 ) ) ;
#21659 = CARTESIAN_POINT ( 'NONE',  ( 37.33957961208646736, -11.81368208888610916, 72.81632618279321889 ) ) ;
#21660 = DIRECTION ( 'NONE',  ( 0.000000000000000000, 1.000000000000000000, -2.999999999999999839E-15 ) ) ;
#21661 = CARTESIAN_POINT ( 'NONE',  ( 38.93415946300898867, -24.11368208888610809, 73.09843995877328382 ) ) ;
#21662 = LINE ( 'NONE', #4016, #10183 ) ;
#21663 = CARTESIAN_POINT ( 'NONE',  ( 39.75915168707251723, 1.096159133578084921, 72.49904802271743165 ) ) ;
#21664 = CARTESIAN_POINT ( 'NONE',  ( 36.31606138205700063, -16.48551471403133206, 77.11349248448009064 ) ) ;
#21665 = EDGE_CURVE ( 'NONE', #6994, #16332, #15088, .T. ) ;
#21666 = CARTESIAN_POINT ( 'NONE',  ( 36.49096545463212493, -21.51368208888609956, 71.43714994484034264 ) ) ;
#21667 = EDGE_CURVE ( 'NONE', #15432, #8317, #2212, .T. ) ;
#21668 = LINE ( 'NONE', #15989, #4502 ) ;
#21669 = EDGE_CURVE ( 'NONE', #17745, #19683, #5243, .T. ) ;
#21670 = AXIS2_PLACEMENT_3D ( 'NONE', #11552, #23248, #19262 ) ;
#21671 = CARTESIAN_POINT ( 'NONE',  ( 36.80608444377001831, -16.30384086642191477, 72.40698646996135324 ) ) ;
#21672 = SPHERICAL_SURFACE ( 'NONE', #21674, 2.000000000000000000 ) ;
#21673 = VECTOR ( 'NONE', #13463, 1000.000000000000000 ) ;
#21674 = AXIS2_PLACEMENT_3D ( 'NONE', #12279, #11898, #2456 ) ;
#21675 = CARTESIAN_POINT ( 'NONE',  ( 38.37017380507020192, -14.01368208888610845, 73.11602215082116629 ) ) ;
#21676 = VERTEX_POINT ( 'NONE', #395 ) ;
#21677 = CARTESIAN_POINT ( 'NONE',  ( 38.37017380507020192, -22.01368208888611022, 73.71602215082113219 ) ) ;
#21678 = VERTEX_POINT ( 'NONE', #19 ) ;
#21679 = PLANE ( 'NONE',  #20561 ) ;
#21680 = DIRECTION ( 'NONE',  ( 0.000000000000000000, 0.7540134720837716742, 0.6568589528324746407 ) ) ;
#21681 = CARTESIAN_POINT ( 'NONE',  ( 37.12184278917507640, -20.10384086642191193, 71.32335560751961623 ) ) ;
#21682 = EDGE_LOOP ( 'NONE', ( #342, #7181, #11918, #19748 ) ) ;
#21683 = VERTEX_POINT ( 'NONE', #9962 ) ;
#21684 = FACE_OUTER_BOUND ( 'NONE', #22633, .T. ) ;
#21685 = DIRECTION ( 'NONE',  ( 0.000000000000000000, -0.8967398287344626739, -0.4425581086832399702 ) ) ;
#21686 = EDGE_CURVE ( 'NONE', #4432, #7783, #152, .T. ) ;
#21687 = CARTESIAN_POINT ( 'NONE',  ( 36.36258059203030513, -27.90384086642191264, 69.89063713639258424 ) ) ;
#21688 = DIRECTION ( 'NONE',  ( 1.000000000000000000, 1.734723475976805122E-16, -1.734723475976811039E-16 ) ) ;
#21689 = CARTESIAN_POINT ( 'NONE',  ( 37.50301148336529167, -1.113682088886101207, 69.06206559358666652 ) ) ;
#21690 = LINE ( 'NONE', #4042, #3200 ) ;
#21691 = VECTOR ( 'NONE', #11110, 1000.000000000000000 ) ;
#21692 = ORIENTED_EDGE ( 'NONE', *, *, #3190, .T. ) ;
#21693 = ORIENTED_EDGE ( 'NONE', *, *, #20104, .F. ) ;
#21694 = CIRCLE ( 'NONE', #4433, 3.000000000000002665 ) ;
#21695 = VECTOR ( 'NONE', #5517, 1000.000000000000000 ) ;
#21696 = CARTESIAN_POINT ( 'NONE',  ( 31.81606138205700418, -34.55876147765400930, 73.30501292737011454 ) ) ;
#21697 = DIRECTION ( 'NONE',  ( -1.000000000000000000, -1.187136597504755470E-16, -8.249087426255173666E-17 ) ) ;
#21698 = CARTESIAN_POINT ( 'NONE',  ( 37.25202387243754032, -24.40384086642191619, 72.75271321436730432 ) ) ;
#21699 = DIRECTION ( 'NONE',  ( 0.000000000000000000, 1.000000000000000000, -2.999999999999999839E-15 ) ) ;
#21700 = ORIENTED_EDGE ( 'NONE', *, *, #2300, .F. ) ;
#21701 = CARTESIAN_POINT ( 'NONE',  ( 37.31606138205700063, 43.19123852234599781, 74.30501292736987295 ) ) ;
#21702 = CYLINDRICAL_SURFACE ( 'NONE', #12764, 1.000000000000000888 ) ;
#21703 = VERTEX_POINT ( 'NONE', #10335 ) ;
#21704 = EDGE_CURVE ( 'NONE', #3835, #21293, #10211, .T. ) ;
#21705 = CARTESIAN_POINT ( 'NONE',  ( 39.31564783533279694, -9.303840866421909439, 70.72433947564853440 ) ) ;
#21706 = EDGE_CURVE ( 'NONE', #5497, #19553, #6347, .T. ) ;
#21707 = LINE ( 'NONE', #182, #14680 ) ;
#21708 = ORIENTED_EDGE ( 'NONE', *, *, #3412, .F. ) ;
#21709 = CARTESIAN_POINT ( 'NONE',  ( 33.31606138205700773, -22.22127907754186893, 75.80501292736997243 ) ) ;
#21710 = ORIENTED_EDGE ( 'NONE', *, *, #3719, .T. ) ;
#21711 = VERTEX_POINT ( 'NONE', #21802 ) ;
#21712 = VECTOR ( 'NONE', #2842, 1000.000000000000114 ) ;
#21713 = DIRECTION ( 'NONE',  ( -1.000000000000000000, -2.999999999999999839E-15, 0.000000000000000000 ) ) ;
#21714 = CARTESIAN_POINT ( 'NONE',  ( 37.38336156205274818, -11.71368208888610241, 72.12822762946750288 ) ) ;
#21715 = VECTOR ( 'NONE', #6483, 1000.000000000000000 ) ;
#21716 = VECTOR ( 'NONE', #13348, 1000.000000000000000 ) ;
#21717 = CARTESIAN_POINT ( 'NONE',  ( 37.69225076346193504, -5.813682088886100274, 72.33091598616827866 ) ) ;
#21718 = VERTEX_POINT ( 'NONE', #23844 ) ;
#21719 = ORIENTED_EDGE ( 'NONE', *, *, #10364, .T. ) ;
#21720 = DIRECTION ( 'NONE',  ( 0.000000000000000000, -0.5706330172266919076, 0.8212051873014208914 ) ) ;
#21721 = CARTESIAN_POINT ( 'NONE',  ( 33.31606138205700773, -27.52349462642295208, 56.67559192035834315 ) ) ;
#21722 = ORIENTED_EDGE ( 'NONE', *, *, #20749, .T. ) ;
#21723 = EDGE_CURVE ( 'NONE', #22871, #17758, #14209, .T. ) ;
#21724 = CARTESIAN_POINT ( 'NONE',  ( 33.56606138205700773, 42.19123852234599781, 75.30501292736987295 ) ) ;
#21725 = CARTESIAN_POINT ( 'NONE',  ( 39.98359781491296161, -17.20384086642190979, 70.89533451361945993 ) ) ;
#21726 = LINE ( 'NONE', #3950, #14888 ) ;
#21727 = DIRECTION ( 'NONE',  ( 0.000000000000000000, -0.8967398287344625629, -0.4425581086832402478 ) ) ;
#21728 = CARTESIAN_POINT ( 'NONE',  ( 38.93987200065208754, -20.81368208888610027, 70.42958956619168021 ) ) ;
#21729 = ORIENTED_EDGE ( 'NONE', *, *, #7371, .T. ) ;
#21730 = VERTEX_POINT ( 'NONE', #9833 ) ;
#21731 = FACE_OUTER_BOUND ( 'NONE', #21466, .T. ) ;
#21732 = CARTESIAN_POINT ( 'NONE',  ( 38.37017380507020192, -12.01368208888610845, 73.11602215082116629 ) ) ;
#21733 = EDGE_CURVE ( 'NONE', #22403, #14130, #10092, .T. ) ;
#21734 = LINE ( 'NONE', #14260, #20909 ) ;
#21735 = FACE_OUTER_BOUND ( 'NONE', #11067, .T. ) ;
#21736 = AXIS2_PLACEMENT_3D ( 'NONE', #17627, #13254, #15170 ) ;
#21737 = CYLINDRICAL_SURFACE ( 'NONE', #24632, 1.000000000000000888 ) ;
#21738 = CARTESIAN_POINT ( 'NONE',  ( 45.81606138205700063, 40.39281886181299797, 82.55501292736983032 ) ) ;
#21739 = DIRECTION ( 'NONE',  ( 1.000000000000000000, 1.185941393278724777E-16, 8.240782279085522416E-17 ) ) ;
#21740 = DIRECTION ( 'NONE',  ( 1.000000000000000000, 1.734723475976804876E-16, -1.734723475976814737E-16 ) ) ;
#21741 = ORIENTED_EDGE ( 'NONE', *, *, #4304, .F. ) ;
#21742 = CARTESIAN_POINT ( 'NONE',  ( 40.31606138205700063, 5.691238522346988127, 65.30501292736998664 ) ) ;
#21743 = ORIENTED_EDGE ( 'NONE', *, *, #18469, .T. ) ;
#21744 = ORIENTED_EDGE ( 'NONE', *, *, #16949, .F. ) ;
#21745 = CARTESIAN_POINT ( 'NONE',  ( 39.12911128074872380, -1.503840866421912725, 69.06206559358666652 ) ) ;
#21746 = VECTOR ( 'NONE', #3646, 1000.000000000000000 ) ;
#21747 = ORIENTED_EDGE ( 'NONE', *, *, #3317, .T. ) ;
#21748 = CARTESIAN_POINT ( 'NONE',  ( 33.31606138205700773, -19.28757846107944474, 24.56123906878952567 ) ) ;
#21749 = CARTESIAN_POINT ( 'NONE',  ( 36.87297107704152666, -7.713682088886109511, 72.49904802271743165 ) ) ;
#21750 = VECTOR ( 'NONE', #5899, 1000.000000000000000 ) ;
#21751 = ORIENTED_EDGE ( 'NONE', *, *, #8457, .T. ) ;
#21752 = DIRECTION ( 'NONE',  ( -1.000000000000000000, 0.000000000000000000, 0.000000000000000000 ) ) ;
#21753 = CARTESIAN_POINT ( 'NONE',  ( 36.36258059203031934, -17.71368208888610596, 72.86986841596736042 ) ) ;
#21754 = EDGE_CURVE ( 'NONE', #9537, #4816, #22049, .T. ) ;
#21755 = AXIS2_PLACEMENT_3D ( 'NONE', #12531, #11090, #10581 ) ;
#21756 = PLANE ( 'NONE',  #11056 ) ;
#21757 = ADVANCED_FACE ( 'NONE', ( #17688 ), #12159, .F. ) ;
#21758 = FACE_OUTER_BOUND ( 'NONE', #24043, .T. ) ;
#21759 = CARTESIAN_POINT ( 'NONE',  ( 43.81606138205700063, 39.55420052130484265, 58.58767820587064534 ) ) ;
#21760 = AXIS2_PLACEMENT_3D ( 'NONE', #6553, #487, #22017 ) ;
#21761 =( NAMED_UNIT ( * ) PLANE_ANGLE_UNIT ( ) SI_UNIT ( $, .RADIAN. ) );
#21762 = CARTESIAN_POINT ( 'NONE',  ( 43.31606138205695089, 3.741517323833267294, 2.753690589366190711 ) ) ;
#21763 = CARTESIAN_POINT ( 'NONE',  ( 32.81606138205700773, 2.191238522347000117, 69.30501292737000085 ) ) ;
#21764 = CARTESIAN_POINT ( 'NONE',  ( 33.31606138205700773, -40.62725863591898445, 68.52362519861142687 ) ) ;
#21765 = CARTESIAN_POINT ( 'NONE',  ( 38.26194895904383486, -23.01368208888610312, 70.24448340153875847 ) ) ;
#21766 = AXIS2_PLACEMENT_3D ( 'NONE', #12939, #1062, #16397 ) ;
#21767 =( BOUNDED_CURVE ( )  B_SPLINE_CURVE ( 3, ( #7307, #11045, #1373, #9259 ),
 .UNSPECIFIED., .F., .T. ) 
 B_SPLINE_CURVE_WITH_KNOTS ( ( 4, 4 ),
 ( 4.712388980384689674, 6.283185307179590673 ),
 .UNSPECIFIED. ) 
 CURVE ( )  GEOMETRIC_REPRESENTATION_ITEM ( )  RATIONAL_B_SPLINE_CURVE ( ( 1.000000000000000000, 0.8047378541243649375, 0.8047378541243649375, 1.000000000000000000 ) ) 
 REPRESENTATION_ITEM ( '' )  );
#21768 = ORIENTED_EDGE ( 'NONE', *, *, #5010, .F. ) ;
#21769 = CARTESIAN_POINT ( 'NONE',  ( 40.52316816324353965, 8.898345303533549355, 69.30501292736998664 ) ) ;
#21770 = ADVANCED_FACE ( 'NONE', ( #18196 ), #7901, .T. ) ;
#21771 = LINE ( 'NONE', #19838, #5765 ) ;
#21772 = ORIENTED_EDGE ( 'NONE', *, *, #7921, .T. ) ;
#21773 = VERTEX_POINT ( 'NONE', #1033 ) ;
#21774 = CARTESIAN_POINT ( 'NONE',  ( 36.36258059203030513, -21.90384086642191619, 69.89063713639259845 ) ) ;
#21775 = VECTOR ( 'NONE', #22015, 1000.000000000000000 ) ;
#21776 = CARTESIAN_POINT ( 'NONE',  ( 39.51027997493896748, -24.51368208888610312, 71.32335560751960202 ) ) ;
#21777 = CARTESIAN_POINT ( 'NONE',  ( 36.36258059203031934, 0.2863179111138938193, 72.86986841596736042 ) ) ;
#21778 = ORIENTED_EDGE ( 'NONE', *, *, #12729, .F. ) ;
#21779 = CARTESIAN_POINT ( 'NONE',  ( 44.81606138205700063, 1.441238522345976714, 67.80501292737001506 ) ) ;
#21780 = CARTESIAN_POINT ( 'NONE',  ( 37.12184278917507640, -0.1038408664219107880, 71.32335560751961623 ) ) ;
#21781 = CIRCLE ( 'NONE', #7812, 4.000000000000000000 ) ;
#21782 = CARTESIAN_POINT ( 'NONE',  ( 29.81606138205707168, -36.80651332587436286, 65.82119181171029254 ) ) ;
#21783 = VERTEX_POINT ( 'NONE', #18569 ) ;
#21784 = DIRECTION ( 'NONE',  ( 1.000000000000000000, 1.734723475976804876E-16, -1.734723475976814737E-16 ) ) ;
#21785 = LINE ( 'NONE', #631, #18654 ) ;
#21786 = CARTESIAN_POINT ( 'NONE',  ( 36.07789103942399578, -2.203840866421915123, 72.05058123536544201 ) ) ;
#21787 = DIRECTION ( 'NONE',  ( -1.000000000000000000, -7.497642437004238434E-16, 3.111695294957277996E-17 ) ) ;
#21788 = VECTOR ( 'NONE', #25094, 1000.000000000000114 ) ;
#21789 = CARTESIAN_POINT ( 'NONE',  ( 46.81606138205695800, -0.7562224151693112129, -1.633662118351544734 ) ) ;
#21790 = CARTESIAN_POINT ( 'NONE',  ( 38.26194895904383486, -5.013682088886102228, 69.64448340153879258 ) ) ;
#21791 = CARTESIAN_POINT ( 'NONE',  ( 33.31606138205697221, -3.118133360756983663, 16.65315793475036443 ) ) ;
#21792 = CARTESIAN_POINT ( 'NONE',  ( 36.87297107704153376, -27.71368208888610596, 72.49904802271738902 ) ) ;
#21793 = VECTOR ( 'NONE', #20923, 1000.000000000000000 ) ;
#21794 = DIRECTION ( 'NONE',  ( 1.000000000000000000, 0.000000000000000000, 0.000000000000000000 ) ) ;
#21795 = CARTESIAN_POINT ( 'NONE',  ( 37.33957961208645315, -1.803840866421907441, 69.94417936956673998 ) ) ;
#21796 = FACE_OUTER_BOUND ( 'NONE', #9189, .T. ) ;
#21797 = VECTOR ( 'NONE', #15517, 1000.000000000000000 ) ;
#21798 = CARTESIAN_POINT ( 'NONE',  ( 37.33957961208646736, -9.813682088886107380, 72.81632618279323310 ) ) ;
#21799 = DIRECTION ( 'NONE',  ( -1.000000000000000000, 0.000000000000000000, 0.000000000000000000 ) ) ;
#21800 = EDGE_CURVE ( 'NONE', #3791, #17124, #270, .T. ) ;
#21801 = CARTESIAN_POINT ( 'NONE',  ( 38.26194895904384907, -10.60384086642191726, 73.11602215082118050 ) ) ;
#21802 = CARTESIAN_POINT ( 'NONE',  ( 44.06606138205700063, 45.04446929126260102, 81.37823623207320622 ) ) ;
#21803 = CARTESIAN_POINT ( 'NONE',  ( 39.38009889167650357, -12.21368208888610596, 72.75271321436731853 ) ) ;
#21804 = ORIENTED_EDGE ( 'NONE', *, *, #4724, .T. ) ;
#21805 = CARTESIAN_POINT ( 'NONE',  ( 40.52078840805428683, -22.61368208888610454, 70.60699637195608602 ) ) ;
#21806 = ORIENTED_EDGE ( 'NONE', *, *, #13047, .F. ) ;
#21807 = CARTESIAN_POINT ( 'NONE',  ( 35.31606138205700773, 7.611641054560886133, 65.67022133066943468 ) ) ;
#21808 = CARTESIAN_POINT ( 'NONE',  ( 32.81606138205700773, -2.088476903695762665, 19.19551655256602984 ) ) ;
#21809 = CARTESIAN_POINT ( 'NONE',  ( 37.38336156205273397, -19.90384086642191264, 70.63227792289247020 ) ) ;
#21810 = VERTEX_POINT ( 'NONE', #2963 ) ;
#21811 = ORIENTED_EDGE ( 'NONE', *, *, #261, .F. ) ;
#21812 = DIRECTION ( 'NONE',  ( 1.000000000000000000, 0.000000000000000000, 0.000000000000000000 ) ) ;
#21813 = DIRECTION ( 'NONE',  ( 0.000000000000000000, -1.000000000000000000, 3.469446951953701358E-15 ) ) ;
#21814 = CARTESIAN_POINT ( 'NONE',  ( 36.07789103942399578, -20.20384086642191335, 72.05058123536544201 ) ) ;
#21815 = VECTOR ( 'NONE', #14727, 1000.000000000000000 ) ;
#21816 = CARTESIAN_POINT ( 'NONE',  ( 39.12911128074873801, -0.1136820888861071882, 73.69843995877330656 ) ) ;
#21817 = DIRECTION ( 'NONE',  ( 0.000000000000000000, -2.999999999999999839E-15, -1.000000000000000000 ) ) ;
#21818 = ORIENTED_EDGE ( 'NONE', *, *, #17196, .F. ) ;
#21819 = ADVANCED_BREP_SHAPE_REPRESENTATION ( '', ( #8398, #2000 ), #6773 ) ;
#21820 = EDGE_LOOP ( 'NONE', ( #17189, #3947, #16258, #3588 ) ) ;
#21821 = LINE ( 'NONE', #12049, #10850 ) ;
#21822 = CARTESIAN_POINT ( 'NONE',  ( 43.81606138205700063, 36.92314894770294131, 80.37823623207323465 ) ) ;
#21823 = CARTESIAN_POINT ( 'NONE',  ( 38.93415946300897446, -21.50384086642190340, 69.66206559358663242 ) ) ;
#21824 = FILL_AREA_STYLE_COLOUR ( '', #20766 ) ;
#21825 = CARTESIAN_POINT ( 'NONE',  ( 44.81606138205700063, 18.19123852234598715, 71.05501292736995822 ) ) ;
#21826 = VERTEX_POINT ( 'NONE', #8533 ) ;
#21827 = AXIS2_PLACEMENT_3D ( 'NONE', #3681, #17606, #13862 ) ;
#21828 = DIRECTION ( 'NONE',  ( 1.000000000000000000, 0.000000000000000000, 0.000000000000000000 ) ) ;
#21829 = EDGE_CURVE ( 'NONE', #3268, #545, #776, .T. ) ;
#21830 = CIRCLE ( 'NONE', #25090, 0.7500000000000001110 ) ;
#21831 = DIRECTION ( 'NONE',  ( -1.000000000000000000, 0.000000000000000000, 0.000000000000000000 ) ) ;
#21832 = EDGE_LOOP ( 'NONE', ( #18414, #14147 ) ) ;
#21833 = CARTESIAN_POINT ( 'NONE',  ( 38.26194895904384197, -4.603840866421910150, 72.51602215082118619 ) ) ;
#21834 = CARTESIAN_POINT ( 'NONE',  ( 32.56606138205700773, 45.04446929126260102, 82.37823623207320622 ) ) ;
#21835 = ORIENTED_EDGE ( 'NONE', *, *, #13175, .F. ) ;
#21836 = FACE_OUTER_BOUND ( 'NONE', #1863, .T. ) ;
#21837 = ORIENTED_EDGE ( 'NONE', *, *, #1540, .F. ) ;
#21838 = ORIENTED_EDGE ( 'NONE', *, *, #8085, .T. ) ;
#21839 = DIRECTION ( 'NONE',  ( 7.071067811865477305E-16, -0.4341746501209515774, -0.9008287146801823297 ) ) ;
#21840 = CARTESIAN_POINT ( 'NONE',  ( 37.38336156205274818, -7.713682088886103294, 72.12822762946751709 ) ) ;
#21841 = CARTESIAN_POINT ( 'NONE',  ( 39.31564783533280405, -6.313682088886101162, 72.03616607671141026 ) ) ;
#21842 = ORIENTED_EDGE ( 'NONE', *, *, #4833, .T. ) ;
#21843 = ORIENTED_EDGE ( 'NONE', *, *, #8465, .T. ) ;
#21844 = DIRECTION ( 'NONE',  ( 1.000000000000000000, 0.000000000000000000, 0.000000000000000000 ) ) ;
#21845 = CARTESIAN_POINT ( 'NONE',  ( 35.56606138205700063, -13.51824891481310509, 37.72654391001022134 ) ) ;
#21846 = CARTESIAN_POINT ( 'NONE',  ( 44.06606138205700063, 45.04446929126260102, 81.37823623207320622 ) ) ;
#21847 = CARTESIAN_POINT ( 'NONE',  ( 36.87297107704149823, -7.903840866421908196, 70.26145752964255564 ) ) ;
#21848 = ADVANCED_FACE ( 'NONE', ( #20247 ), #14325, .T. ) ;
#21849 = ADVANCED_FACE ( 'NONE', ( #22178 ), #4662, .F. ) ;
#21850 = CIRCLE ( 'NONE', #9525, 1.099999999999998312 ) ;
#21851 = LINE ( 'NONE', #6735, #2945 ) ;
#21852 = CARTESIAN_POINT ( 'NONE',  ( 40.81606138205700773, -31.05876147765399864, 75.30501292737010033 ) ) ;
#21853 = DIRECTION ( 'NONE',  ( -8.552847072295029957E-47, 1.000000000000000000, -2.999999999999999839E-15 ) ) ;
#21854 = EDGE_CURVE ( 'NONE', #2100, #14645, #20446, .T. ) ;
#21855 = ORIENTED_EDGE ( 'NONE', *, *, #14600, .F. ) ;
#21856 = AXIS2_PLACEMENT_3D ( 'NONE', #11172, #3163, #6915 ) ;
#21857 = ADVANCED_FACE ( 'NONE', ( #24342 ), #6468, .F. ) ;
#21858 = EDGE_CURVE ( 'NONE', #16039, #1577, #6592, .T. ) ;
#21859 = VERTEX_POINT ( 'NONE', #5040 ) ;
#21860 = DIRECTION ( 'NONE',  ( 1.000000000000000000, 0.000000000000000000, 0.000000000000000000 ) ) ;
#21861 = CARTESIAN_POINT ( 'NONE',  ( 38.26194895904383486, -13.01368208888610134, 69.64448340153877837 ) ) ;
#21862 = CARTESIAN_POINT ( 'NONE',  ( 33.31606138205700773, -32.95845724189726411, 59.23979596822106686 ) ) ;
#21863 = DIRECTION ( 'NONE',  ( 0.000000000000000000, 6.938893903907222067E-15, -1.000000000000000000 ) ) ;
#21864 = CARTESIAN_POINT ( 'NONE',  ( 30.81606138205700418, 40.83281886181300280, 78.30501292736983032 ) ) ;
#21865 = DIRECTION ( 'NONE',  ( 0.000000000000000000, 0.5706330172266919076, -0.8212051873014208914 ) ) ;
#21866 = ADVANCED_FACE ( 'NONE', ( #903, #6715 ), #648, .F. ) ;
#21867 = PRODUCT_DEFINITION_SHAPE ( 'NONE', 'NONE',  #25194 ) ;
#21868 = EDGE_CURVE ( 'NONE', #23317, #25393, #20377, .T. ) ;
#21869 = DIRECTION ( 'NONE',  ( 0.000000000000000000, -1.000000000000000000, 3.491481338843134933E-15 ) ) ;
#21870 = DIRECTION ( 'NONE',  ( 0.000000000000000000, 1.000000000000000000, 0.000000000000000000 ) ) ;
#21871 = VERTEX_POINT ( 'NONE', #16368 ) ;
#21872 = DIRECTION ( 'NONE',  ( 0.000000000000000000, -1.000000000000000000, 3.129456975819164530E-15 ) ) ;
#21873 = ORIENTED_EDGE ( 'NONE', *, *, #15538, .T. ) ;
#21874 = ORIENTED_EDGE ( 'NONE', *, *, #11159, .T. ) ;
#21875 = FACE_OUTER_BOUND ( 'NONE', #24418, .T. ) ;
#21876 = CARTESIAN_POINT ( 'NONE',  ( 36.98690846071097127, -3.803840866421912992, 69.45876917294177133 ) ) ;
#21877 = VERTEX_POINT ( 'NONE', #4781 ) ;
#21878 = EDGE_CURVE ( 'NONE', #13976, #3066, #12658, .T. ) ;
#21879 = STYLED_ITEM ( 'NONE', ( #1936 ), #17330 ) ;
#21880 = LINE ( 'NONE', #19684, #16118 ) ;
#21881 = CARTESIAN_POINT ( 'NONE',  ( 40.14115730948191185, -6.513682088886103116, 71.32335560751961623 ) ) ;
#21882 = ORIENTED_EDGE ( 'NONE', *, *, #18218, .F. ) ;
#21883 = PLANE ( 'NONE',  #17392 ) ;
#21884 = CARTESIAN_POINT ( 'NONE',  ( 38.26194895904383486, -13.01368208888610312, 69.04448340153878405 ) ) ;
#21885 = CARTESIAN_POINT ( 'NONE',  ( 42.82259773799690805, 3.224889347397511763, 6.370942022298698326 ) ) ;
#21886 = DIRECTION ( 'NONE',  ( 0.000000000000000000, 1.000000000000000000, -3.469446951953613400E-15 ) ) ;
#21887 = VECTOR ( 'NONE', #9511, 1000.000000000000000 ) ;
#21888 = AXIS2_PLACEMENT_3D ( 'NONE', #22007, #20577, #8740 ) ;
#21889 = CARTESIAN_POINT ( 'NONE',  ( 43.31331964531621281, 4.015598734371947032, 6.338464250156571111 ) ) ;
#21890 = LINE ( 'NONE', #18036, #25455 ) ;
#21891 = AXIS2_PLACEMENT_3D ( 'NONE', #22121, #469, #10155 ) ;
#21892 = FACE_OUTER_BOUND ( 'NONE', #1216, .T. ) ;
#21893 = DIRECTION ( 'NONE',  ( -1.000000000000000000, -1.187136597504755470E-16, -8.249087426255172434E-17 ) ) ;
#21894 = CARTESIAN_POINT ( 'NONE',  ( 38.73920764526925353, -24.11368208888610098, 72.49843995877328950 ) ) ;
#21895 = EDGE_LOOP ( 'NONE', ( #10237, #6381, #798, #24132 ) ) ;
#21896 = CARTESIAN_POINT ( 'NONE',  ( 40.26527270485448184, -20.81444828448985973, 75.91197220037939530 ) ) ;
#21897 = LINE ( 'NONE', #6558, #17720 ) ;
#21898 = ORIENTED_EDGE ( 'NONE', *, *, #2098, .F. ) ;
#21899 = ORIENTED_EDGE ( 'NONE', *, *, #15190, .F. ) ;
#21900 = CARTESIAN_POINT ( 'NONE',  ( 36.11133435605973574, -24.00384086642191761, 70.60699637195608602 ) ) ;
#21901 = PRODUCT_DEFINITION ( 'UNKNOWN', '', #21170, #4385 ) ;
#21902 = CARTESIAN_POINT ( 'NONE',  ( 36.89935272106204422, 0.7863179111138978161, 69.52238214136768590 ) ) ;
#21903 = DIRECTION ( 'NONE',  ( -1.000000000000000000, 0.000000000000000000, 0.000000000000000000 ) ) ;
#21904 = CIRCLE ( 'NONE', #11639, 4.000000000000000000 ) ;
#21905 = ORIENTED_EDGE ( 'NONE', *, *, #15631, .F. ) ;
#21906 = FACE_OUTER_BOUND ( 'NONE', #12379, .T. ) ;
#21907 = FACE_OUTER_BOUND ( 'NONE', #18666, .T. ) ;
#21908 = VECTOR ( 'NONE', #6258, 1000.000000000000114 ) ;
#21909 = CARTESIAN_POINT ( 'NONE',  ( 39.02088643472237806, -2.703840866421919120, 73.73360434286902887 ) ) ;
#21910 = CYLINDRICAL_SURFACE ( 'NONE', #14409, 1.250000000000000888 ) ;
#21911 = FACE_OUTER_BOUND ( 'NONE', #16366, .T. ) ;
#21912 = CARTESIAN_POINT ( 'NONE',  ( 36.64852494920107517, -7.413682088886104360, 70.89533451361948835 ) ) ;
#21913 = CARTESIAN_POINT ( 'NONE',  ( 46.91606138205695231, -23.19619402982945644, 47.16846523730003327 ) ) ;
#21914 = VECTOR ( 'NONE', #480, 1000.000000000000000 ) ;
#21915 = AXIS2_PLACEMENT_3D ( 'NONE', #3582, #25211, #19688 ) ;
#21916 = CARTESIAN_POINT ( 'NONE',  ( 37.33957961208646736, -25.81368208888610738, 72.81632618279320468 ) ) ;
#21917 = DIRECTION ( 'NONE',  ( 0.000000000000000000, -3.965082230804126670E-15, -1.000000000000000000 ) ) ;
#21918 = AXIS2_PLACEMENT_3D ( 'NONE', #23763, #6627, #16409 ) ;
#21919 = CARTESIAN_POINT ( 'NONE',  ( 39.38009889167648936, 0.5961591335780919154, 70.00779233799265455 ) ) ;
#21920 = VECTOR ( 'NONE', #2359, 1000.000000000000000 ) ;
#21921 = CARTESIAN_POINT ( 'NONE',  ( 40.31606138205700773, -13.58280000135113319, 20.54174511886706256 ) ) ;
#21922 = CARTESIAN_POINT ( 'NONE',  ( 38.00113996487112189, -23.70384086642191335, 70.22690120949089021 ) ) ;
#21923 = CARTESIAN_POINT ( 'NONE',  ( 37.25202387243752611, -15.21368208888610063, 70.00779233799262613 ) ) ;
#21924 = FACE_OUTER_BOUND ( 'NONE', #24794, .T. ) ;
#21925 = VECTOR ( 'NONE', #25400, 1000.000000000000000 ) ;
#21926 = EDGE_CURVE ( 'NONE', #23160, #17369, #15918, .T. ) ;
#21927 = CARTESIAN_POINT ( 'NONE',  ( 38.93415946300896024, -13.50384086642190518, 69.66206559358661821 ) ) ;
#21928 = DIRECTION ( 'NONE',  ( -0.1733269559585509378, 0.000000000000000000, -0.9848643390529188135 ) ) ;
#21929 = AXIS2_PLACEMENT_3D ( 'NONE', #10651, #18500, #6899 ) ;
#21930 = CARTESIAN_POINT ( 'NONE',  ( 36.68196826583682935, -11.61368208888610276, 71.96809898377888715 ) ) ;
#21931 = ORIENTED_EDGE ( 'NONE', *, *, #17303, .T. ) ;
#21932 = CARTESIAN_POINT ( 'NONE',  ( 39.64521430340304420, -14.81368208888610205, 69.45876917294175712 ) ) ;
#21933 = ORIENTED_EDGE ( 'NONE', *, *, #16168, .T. ) ;
#21934 = FACE_OUTER_BOUND ( 'NONE', #5654, .T. ) ;
#21935 = CARTESIAN_POINT ( 'NONE',  ( 30.81606138205700418, 40.39281886181299797, 82.55501292736983032 ) ) ;
#21936 = CARTESIAN_POINT ( 'NONE',  ( 39.02742774030101458, -17.40384086642191264, 70.49320253461759478 ) ) ;
#21937 = ORIENTED_EDGE ( 'NONE', *, *, #23909, .T. ) ;
#21938 = ORIENTED_EDGE ( 'NONE', *, *, #23090, .T. ) ;
#21939 = CARTESIAN_POINT ( 'NONE',  ( 30.81606138205698642, -6.548589660139424673, -8.069948661059610728 ) ) ;
#21940 = CARTESIAN_POINT ( 'NONE',  ( 36.31606138205700063, -10.93995761290683255, 80.99653337025984001 ) ) ;
#21941 = CARTESIAN_POINT ( 'NONE',  ( 36.29569395875881099, -24.30384086642192187, 72.77780686321126780 ) ) ;
#21942 = CIRCLE ( 'NONE', #1357, 10.00000000000000000 ) ;
#21943 = CARTESIAN_POINT ( 'NONE',  ( 42.06606138205700063, 41.44123852234599781, 74.30501292736987295 ) ) ;
#21944 = CARTESIAN_POINT ( 'NONE',  ( 36.87297107704152666, -23.71368208888610951, 72.49904802271738902 ) ) ;
#21945 = EDGE_CURVE ( 'NONE', #16500, #22610, #20500, .T. ) ;
#21946 = CARTESIAN_POINT ( 'NONE',  ( 33.56606138205700773, 42.19123852234601202, 79.18605660143489899 ) ) ;
#21947 = ORIENTED_EDGE ( 'NONE', *, *, #3353, .T. ) ;
#21948 = ORIENTED_EDGE ( 'NONE', *, *, #3730, .F. ) ;
#21949 = CARTESIAN_POINT ( 'NONE',  ( 44.81606138205700063, -11.72563467517899838, 72.98595903681223263 ) ) ;
#21950 = LINE ( 'NONE', #4181, #10997 ) ;
#21951 = AXIS2_PLACEMENT_3D ( 'NONE', #13967, #4312, #13718 ) ;
#21952 = CARTESIAN_POINT ( 'NONE',  ( 38.37017380507018771, -23.60384086642190837, 69.64448340153877837 ) ) ;
#21953 = LINE ( 'NONE', #9986, #5896 ) ;
#21954 = ORIENTED_EDGE ( 'NONE', *, *, #1302, .T. ) ;
#21955 = PRESENTATION_LAYER_ASSIGNMENT (  '', '', ( #22363 ) ) ;
#21956 = PLANE ( 'NONE',  #14760 ) ;
#21957 = AXIS2_PLACEMENT_3D ( 'NONE', #11031, #22137, #6433 ) ;
#21958 = CARTESIAN_POINT ( 'NONE',  ( 41.81606138205696510, -0.1886652901601590937, -3.819484830245897911 ) ) ;
#21959 = CARTESIAN_POINT ( 'NONE',  ( 39.51027997493896748, -1.103840866421911704, 71.43714994484034264 ) ) ;
#21960 = DIRECTION ( 'NONE',  ( -4.256992727861094749E-32, 1.000000000000000000, -3.115648231731786715E-15 ) ) ;
#21961 = ORIENTED_EDGE ( 'NONE', *, *, #2147, .T. ) ;
#21962 = AXIS2_PLACEMENT_3D ( 'NONE', #3976, #12589, #10517 ) ;
#21963 = CARTESIAN_POINT ( 'NONE',  ( 39.29254315202756231, -28.81368208888610383, 69.94417936956671156 ) ) ;
#21964 = ORIENTED_EDGE ( 'NONE', *, *, #8608, .F. ) ;
#21965 = ORIENTED_EDGE ( 'NONE', *, *, #128, .T. ) ;
#21966 = CARTESIAN_POINT ( 'NONE',  ( 45.81606138205700063, -38.55876147765410167, 72.21586839016147508 ) ) ;
#21967 = DIRECTION ( 'NONE',  ( 1.000000000000000000, 0.000000000000000000, 0.000000000000000000 ) ) ;
#21968 = CARTESIAN_POINT ( 'NONE',  ( 39.31564783533280405, -8.313682088886102051, 72.03616607671141026 ) ) ;
#21969 = CARTESIAN_POINT ( 'NONE',  ( 37.38336156205274818, -5.713682088886101518, 72.12822762946751709 ) ) ;
#21970 = ORIENTED_EDGE ( 'NONE', *, *, #23908, .F. ) ;
#21971 = ORIENTED_EDGE ( 'NONE', *, *, #10975, .F. ) ;
#21972 = DIRECTION ( 'NONE',  ( 0.000000000000000000, 1.000000000000000000, -3.469446951953614189E-15 ) ) ;
#21973 = DIRECTION ( 'NONE',  ( 0.000000000000000000, 0.7071067811865455743, 0.7071067811865494601 ) ) ;
#21974 = CYLINDRICAL_SURFACE ( 'NONE', #5412, 0.7500000000000006661 ) ;
#21975 = CARTESIAN_POINT ( 'NONE',  ( 38.93415946300896024, -13.50384086642190518, 69.66206559358661821 ) ) ;
#21976 = APPLICATION_CONTEXT ( 'automotive_design' ) ;
#21977 = COLOUR_RGB ( '', 0.31764706, 0.68627451, 0.89019608) ;
#21978 = CARTESIAN_POINT ( 'NONE',  ( 44.81606138205700063, 41.44123852234596939, 66.30501292736988717 ) ) ;
#21979 = EDGE_CURVE ( 'NONE', #5370, #6126, #7709, .T. ) ;
#21980 = DIRECTION ( 'NONE',  ( 0.000000000000000000, -2.999999999999999839E-15, -1.000000000000000000 ) ) ;
#21981 = ORIENTED_EDGE ( 'NONE', *, *, #14272, .F. ) ;
#21982 = VECTOR ( 'NONE', #7147, 1000.000000000000000 ) ;
#21983 = AXIS2_PLACEMENT_3D ( 'NONE', #18862, #10632, #16535 ) ;
#21984 = ORIENTED_EDGE ( 'NONE', *, *, #7129, .T. ) ;
#21985 = ORIENTED_EDGE ( 'NONE', *, *, #17919, .F. ) ;
#21986 = CARTESIAN_POINT ( 'NONE',  ( 28.84183937708599998, -34.55876147765400219, 70.30501292737000085 ) ) ;
#21987 = CARTESIAN_POINT ( 'NONE',  ( 39.98359781491296161, -6.413682088886103472, 71.86517103874048473 ) ) ;
#21988 =( GEOMETRIC_REPRESENTATION_CONTEXT ( 3 ) GLOBAL_UNCERTAINTY_ASSIGNED_CONTEXT ( ( #4069 ) ) GLOBAL_UNIT_ASSIGNED_CONTEXT ( ( #4040, #17324, #17577 ) ) REPRESENTATION_CONTEXT ( 'NONE', 'WORKASPACE' ) );
#21989 = FACE_OUTER_BOUND ( 'NONE', #21385, .T. ) ;
#21990 = FACE_BOUND ( 'NONE', #25233, .T. ) ;
#21991 = CARTESIAN_POINT ( 'NONE',  ( 38.31606138205692247, 12.90996180647746350, 7.674666182279729298 ) ) ;
#21992 = CARTESIAN_POINT ( 'NONE',  ( 40.05245289102396100, -29.10876147765230115, 71.40796565871902146 ) ) ;
#21993 = CARTESIAN_POINT ( 'NONE',  ( 36.31606138205698642, -9.092667827980706718, 28.75914562266559926 ) ) ;
#21994 = PLANE ( 'NONE',  #8571 ) ;
#21995 = EDGE_CURVE ( 'NONE', #20600, #9497, #12786, .T. ) ;
#21996 = EDGE_CURVE ( 'NONE', #15888, #8849, #18698, .T. ) ;
#21997 = DIRECTION ( 'NONE',  ( 1.000000000000000000, 0.000000000000000000, 0.000000000000000000 ) ) ;
#21998 = EDGE_LOOP ( 'NONE', ( #1918, #8896, #17241, #23100 ) ) ;
#21999 = EDGE_CURVE ( 'NONE', #7140, #24390, #3096, .T. ) ;
#22000 = EDGE_LOOP ( 'NONE', ( #17989, #13482, #3148, #10139 ) ) ;
#22001 = VECTOR ( 'NONE', #9318, 1000.000000000000000 ) ;
#22002 = FACE_OUTER_BOUND ( 'NONE', #23628, .T. ) ;
#22003 = CARTESIAN_POINT ( 'NONE',  ( 39.73277004305197124, -7.403840866421910860, 69.52238214136768590 ) ) ;
#22004 = EDGE_CURVE ( 'NONE', #13614, #22981, #20960, .T. ) ;
#22005 = EDGE_CURVE ( 'NONE', #1363, #4055, #5178, .T. ) ;
#22006 = VERTEX_POINT ( 'NONE', #1159 ) ;
#22007 = CARTESIAN_POINT ( 'NONE',  ( 44.81606138205700063, 2.788239579249953820E-13, 80.37823623207336254 ) ) ;
#22008 = CARTESIAN_POINT ( 'NONE',  ( 37.33957961208646736, -5.813682088886107380, 72.81632618279323310 ) ) ;
#22009 = DIRECTION ( 'NONE',  ( 2.690219486203388234E-15, -0.8967398287344627850, -0.4425581086832399147 ) ) ;
#22010 = EDGE_CURVE ( 'NONE', #8578, #18480, #25458, .T. ) ;
#22011 = CARTESIAN_POINT ( 'NONE',  ( 39.12911128074873801, -18.11368208888610454, 73.69843995877327814 ) ) ;
#22012 = DIRECTION ( 'NONE',  ( -1.327674326049719602E-15, 0.4425581086832399147, -0.8967398287344627850 ) ) ;
#22013 = DIRECTION ( 'NONE',  ( -1.000000000000000000, -1.734723475976804876E-16, 1.734723475976814737E-16 ) ) ;
#22014 = DIRECTION ( 'NONE',  ( 0.000000000000000000, 1.000000000000000000, 0.000000000000000000 ) ) ;
#22015 = DIRECTION ( 'NONE',  ( 1.000000000000000000, 0.000000000000000000, 0.000000000000000000 ) ) ;
#22016 = DIRECTION ( 'NONE',  ( 1.000000000000000000, 1.734723475976804876E-16, -1.734723475976814737E-16 ) ) ;
#22017 = DIRECTION ( 'NONE',  ( 0.000000000000000000, -1.000000000000000000, 2.999999999999999839E-15 ) ) ;
#22018 = CARTESIAN_POINT ( 'NONE',  ( 38.63098279924288647, -24.91368208888610170, 70.22690120949089021 ) ) ;
#22019 = ORIENTED_EDGE ( 'NONE', *, *, #23492, .F. ) ;
#22020 = CARTESIAN_POINT ( 'NONE',  ( 40.05426416818898616, -21.21860219669770231, 75.34973409106177655 ) ) ;
#22021 = LINE ( 'NONE', #2554, #1253 ) ;
#22022 = VERTEX_POINT ( 'NONE', #3358 ) ;
#22023 = VERTEX_POINT ( 'NONE', #16894 ) ;
#22024 = CARTESIAN_POINT ( 'NONE',  ( 39.02088643472237806, -26.70384086642192401, 73.73360434286898624 ) ) ;
#22025 = EDGE_CURVE ( 'NONE', #4126, #16336, #11084, .T. ) ;
#22026 = ADVANCED_FACE ( 'NONE', ( #9309 ), #11100, .T. ) ;
#22027 = CARTESIAN_POINT ( 'NONE',  ( 39.29254315202756231, -24.81368208888610383, 69.94417936956671156 ) ) ;
#22028 = DIRECTION ( 'NONE',  ( 0.9835979625596965592, -0.1803747433772641684, -2.086002012065537230E-15 ) ) ;
#22029 = CIRCLE ( 'NONE', #23254, 2.000000000000001776 ) ;
#22030 = CARTESIAN_POINT ( 'NONE',  ( 32.31606138205700063, -20.93319939328399926, 43.78741072286599945 ) ) ;
#22031 = ORIENTED_EDGE ( 'NONE', *, *, #5849, .T. ) ;
#22032 = FACE_OUTER_BOUND ( 'NONE', #23450, .T. ) ;
#22033 = DIRECTION ( 'NONE',  ( -1.000000000000000000, 0.000000000000000000, 0.000000000000000000 ) ) ;
#22034 = ADVANCED_FACE ( 'NONE', ( #9052 ), #9179, .T. ) ;
#22035 = CARTESIAN_POINT ( 'NONE',  ( 36.07789103942399578, -6.203840866421916900, 72.05058123536544201 ) ) ;
#22036 = CARTESIAN_POINT ( 'NONE',  ( 38.41621794735363693, -36.60729675983900222, 84.30501292737011454 ) ) ;
#22037 = CARTESIAN_POINT ( 'NONE',  ( 44.31606138205700063, 10.62769494289597993, 68.29765714199933768 ) ) ;
#22038 = CARTESIAN_POINT ( 'NONE',  ( 37.80618814713140097, -9.913682088886107024, 73.13360434286904876 ) ) ;
#22039 = DIRECTION ( 'NONE',  ( 1.000000000000000000, 0.000000000000000000, 0.000000000000000000 ) ) ;
#22040 = CARTESIAN_POINT ( 'NONE',  ( 39.59324923284151510, -28.74115096347518161, 70.20355626897213597 ) ) ;
#22041 = CARTESIAN_POINT ( 'NONE',  ( 31.81606138205700418, 38.19123852234599070, 72.05501292736988717 ) ) ;
#22042 = EDGE_CURVE ( 'NONE', #16336, #9479, #11234, .T. ) ;
#22043 = DIRECTION ( 'NONE',  ( -1.000000000000000000, -3.046270958365671426E-15, 5.272995181423179347E-17 ) ) ;
#22044 = DIRECTION ( 'NONE',  ( 0.000000000000000000, 0.3299742535180974490, -0.9439899321577398528 ) ) ;
#22045 = CARTESIAN_POINT ( 'NONE',  ( 37.60469502381300799, -24.40384086642190908, 72.26730301774232146 ) ) ;
#22046 = CARTESIAN_POINT ( 'NONE',  ( 37.80618814713140097, -13.91368208888610347, 73.13360434286903455 ) ) ;
#22047 = FACE_OUTER_BOUND ( 'NONE', #22657, .T. ) ;
#22048 = CARTESIAN_POINT ( 'NONE',  ( 37.25202387243754032, -14.40384086642191619, 72.75271321436731853 ) ) ;
#22049 = LINE ( 'NONE', #12029, #24937 ) ;
#22050 = CARTESIAN_POINT ( 'NONE',  ( 39.29254315202756231, -12.81368208888610383, 69.94417936956672577 ) ) ;
#22051 = ORIENTED_EDGE ( 'NONE', *, *, #13196, .F. ) ;
#22052 = CARTESIAN_POINT ( 'NONE',  ( 39.73277004305198545, -14.21368208888610951, 73.23812341099225875 ) ) ;
#22053 = ORIENTED_EDGE ( 'NONE', *, *, #14281, .F. ) ;
#22054 = DIRECTION ( 'NONE',  ( -1.000000000000000000, 0.000000000000000000, 0.000000000000000000 ) ) ;
#22055 = DIRECTION ( 'NONE',  ( 0.000000000000000000, 0.000000000000000000, 1.000000000000000000 ) ) ;
#22056 = CARTESIAN_POINT ( 'NONE',  ( 39.02742774030101458, -19.40384086642191264, 70.49320253461759478 ) ) ;
#22057 = EDGE_LOOP ( 'NONE', ( #10544, #10015, #9113, #14448 ) ) ;
#22058 = ORIENTED_EDGE ( 'NONE', *, *, #23592, .F. ) ;
#22059 = DIRECTION ( 'NONE',  ( -1.734723475976804876E-16, -3.491481338843135327E-15, -1.000000000000000000 ) ) ;
#22060 = CARTESIAN_POINT ( 'NONE',  ( 38.14273442609844977, 40.69123852234599781, 70.32014858831708182 ) ) ;
#22061 = CARTESIAN_POINT ( 'NONE',  ( 36.89935272106205133, -22.40384086642191974, 73.23812341099225875 ) ) ;
#22062 = CARTESIAN_POINT ( 'NONE',  ( 40.31606138205700773, -31.05876147765400574, 73.55501292737010033 ) ) ;
#22063 = CARTESIAN_POINT ( 'NONE',  ( 36.68196826583682935, -25.61368208888610454, 71.96809898377887293 ) ) ;
#22064 = PRODUCT_DEFINITION_SHAPE ( 'NONE', 'NONE',  #25491 ) ;
#22065 = DIRECTION ( 'NONE',  ( -1.123589211228918605E-15, 0.4425581086832399147, -0.8967398287344627850 ) ) ;
#22066 = EDGE_CURVE ( 'NONE', #23642, #17124, #10171, .T. ) ;
#22067 = ORIENTED_EDGE ( 'NONE', *, *, #17366, .F. ) ;
#22068 = ADVANCED_FACE ( 'NONE', ( #357 ), #12373, .F. ) ;
#22069 = DIRECTION ( 'NONE',  ( 0.000000000000000000, -0.5706330172267045642, 0.8212051873014122316 ) ) ;
#22070 = DIRECTION ( 'NONE',  ( 0.000000000000000000, -0.6568589528324746407, 0.7540134720837717852 ) ) ;
#22071 = ADVANCED_FACE ( 'NONE', ( #2423 ), #4626, .F. ) ;
#22072 = CARTESIAN_POINT ( 'NONE',  ( 36.68196826583682935, -14.00384086642191228, 70.79240656858107172 ) ) ;
#22073 =( NAMED_UNIT ( * ) SI_UNIT ( $, .STERADIAN. ) SOLID_ANGLE_UNIT ( ) );
#22074 = DIRECTION ( 'NONE',  ( -1.734723475976879818E-16, 1.000000000000000000, -4.343580702399009298E-14 ) ) ;
#22075 = ORIENTED_EDGE ( 'NONE', *, *, #23237, .T. ) ;
#22076 = LINE ( 'NONE', #17851, #3237 ) ;
#22077 = DIRECTION ( 'NONE',  ( 1.510383499235849534E-16, 0.1218693434051499741, 0.9925461516413217611 ) ) ;
#22078 = CARTESIAN_POINT ( 'NONE',  ( 38.73920764526923932, 0.4961591335780889955, 70.26206559358665515 ) ) ;
#22079 = DIRECTION ( 'NONE',  ( -0.1733269559585477460, -5.551115123125804790E-15, -0.9848643390529193686 ) ) ;
#22080 = ORIENTED_EDGE ( 'NONE', *, *, #24203, .T. ) ;
#22081 = EDGE_CURVE ( 'NONE', #11945, #20798, #616, .T. ) ;
#22082 = CARTESIAN_POINT ( 'NONE',  ( 35.81606138205700063, -29.78523130861184498, 52.92072663988442116 ) ) ;
#22083 = VERTEX_POINT ( 'NONE', #10300 ) ;
#22084 = EDGE_LOOP ( 'NONE', ( #18426, #16130, #14004, #23895 ) ) ;
#22085 = CARTESIAN_POINT ( 'NONE',  ( 46.81606138205697221, -3.227578639999799659, -4.500312080287595329 ) ) ;
#22086 = CYLINDRICAL_SURFACE ( 'NONE', #10816, 1.000000000000000888 ) ;
#22087 = UNCERTAINTY_MEASURE_WITH_UNIT (LENGTH_MEASURE( 1.000000000000000082E-05 ), #7632, 'distance_accuracy_value', 'NONE');
#22088 = CARTESIAN_POINT ( 'NONE',  ( 37.31647492878122563, -3.313682088886101607, 70.72433947564853440 ) ) ;
#22089 = CARTESIAN_POINT ( 'NONE',  ( 38.93987200065208754, -6.813682088886101162, 70.42958956619168021 ) ) ;
#22090 = ORIENTED_EDGE ( 'NONE', *, *, #25431, .T. ) ;
#22091 = VERTEX_POINT ( 'NONE', #23936 ) ;
#22092 = CARTESIAN_POINT ( 'NONE',  ( 33.48677699869404023, 3.517612739349352591, 6.329933951274631099 ) ) ;
#22093 = DIRECTION ( 'NONE',  ( 0.000000000000000000, -1.000000000000000000, 6.938893903907222067E-15 ) ) ;
#22094 = VERTEX_POINT ( 'NONE', #20213 ) ;
#22095 = CARTESIAN_POINT ( 'NONE',  ( 43.31606138205700063, -2.088476903695762665, 19.19551655256602984 ) ) ;
#22096 = CARTESIAN_POINT ( 'NONE',  ( 39.95015449827720744, -11.00384086642191050, 71.96809898377888715 ) ) ;
#22097 = AXIS2_PLACEMENT_3D ( 'NONE', #9070, #19103, #1441 ) ;
#22098 = AXIS2_PLACEMENT_3D ( 'NONE', #16549, #3279, #6894 ) ;
#22099 = AXIS2_PLACEMENT_3D ( 'NONE', #20271, #6110, #13969 ) ;
#22100 = AXIS2_PLACEMENT_3D ( 'NONE', #6840, #14695, #22559 ) ;
#22101 = DIRECTION ( 'NONE',  ( 1.000000000000000000, 2.954840238787252245E-15, 9.150562545582958565E-17 ) ) ;
#22102 = FACE_OUTER_BOUND ( 'NONE', #13199, .T. ) ;
#22103 = ORIENTED_EDGE ( 'NONE', *, *, #6897, .F. ) ;
#22104 = VERTEX_POINT ( 'NONE', #6311 ) ;
#22105 = ORIENTED_EDGE ( 'NONE', *, *, #6273, .T. ) ;
#22106 = DIRECTION ( 'NONE',  ( 0.000000000000000000, 0.9992330079037401447, -0.03915859951075795903 ) ) ;
#22107 = CARTESIAN_POINT ( 'NONE',  ( 39.95015449827720744, -8.613682088886104538, 70.79240656858107172 ) ) ;
#22108 = CARTESIAN_POINT ( 'NONE',  ( 44.81606138205700063, -34.55876147765410167, 70.30501292737000085 ) ) ;
#22109 = PLANE ( 'NONE',  #12046 ) ;
#22110 = CARTESIAN_POINT ( 'NONE',  ( 44.81606138205700063, 0.1601050959395486362, 68.80395113470939350 ) ) ;
#22111 = LINE ( 'NONE', #11835, #20494 ) ;
#22112 = CLOSED_SHELL ( 'NONE', ( #748, #8623, #13848, #3901, #24411, #12962, #6487, #3386, #10005, #11959, #1053, #2558, #10362, #3824, #5850, #9115, #6657, #19963, #14870, #24702, #22861, #14285, #15308, #25100, #1034, #6101, #15009, #4676, #8856, #5958, #20686, #1274, #25293, #3754, #7847, #22323, #24824, #21615, #2130, #16675, #11259, #19434, #2649, #2344, #4778, #7507, #7225, #5003, #22335, #13356, #24975, #6281, #11711, #23743, #2478, #5943, #14115, #19867, #1728, #17959, #20990, #1071, #1160, #8297, #886, #18138, #17289, #15067, #14887, #24034, #749, #1758, #9030, #20573, #11601, #4231, #25285, #18139, #16055, #16722, #7992, #4248, #2762, #1043, #6588, #25306, #13735, #24685, #8488, #17532, #430, #23306, #8303, #18304, #10690, #16188, #25291, #19637, #579, #13838, #15270, #24994 ) ) ;
#22113 = CARTESIAN_POINT ( 'NONE',  ( 36.31606138205700063, -30.30876147765401996, 69.30501292737010033 ) ) ;
#22114 = DIRECTION ( 'NONE',  ( 0.000000000000000000, -1.000000000000000000, 2.999999999999999839E-15 ) ) ;
#22115 = CIRCLE ( 'NONE', #24155, 1.100000000000000311 ) ;
#22116 = CIRCLE ( 'NONE', #24958, 1.800000000000002931 ) ;
#22117 = ADVANCED_FACE ( 'NONE', ( #24181 ), #10054, .F. ) ;
#22118 = CARTESIAN_POINT ( 'NONE',  ( 37.25504499466181585, -21.91763188072224011, 75.30955569975962760 ) ) ;
#22119 = ORIENTED_EDGE ( 'NONE', *, *, #4232, .T. ) ;
#22120 = ORIENTED_EDGE ( 'NONE', *, *, #22816, .F. ) ;
#22121 = CARTESIAN_POINT ( 'NONE',  ( 32.81606138205700773, -37.34243788671330577, 70.80615726751818784 ) ) ;
#22122 = CARTESIAN_POINT ( 'NONE',  ( 38.37017380507018771, -7.603840866421910150, 69.04448340153881247 ) ) ;
#22123 = ORIENTED_EDGE ( 'NONE', *, *, #13097, .F. ) ;
#22124 = CARTESIAN_POINT ( 'NONE',  ( 44.81606138205700063, -34.55876147765410167, 70.30501292737000085 ) ) ;
#22125 = CARTESIAN_POINT ( 'NONE',  ( 39.75915168707250302, -10.71368208888609885, 70.26145752964252722 ) ) ;
#22126 = CARTESIAN_POINT ( 'NONE',  ( 39.31606138205700063, 43.19123852234599781, 74.30501292736987295 ) ) ;
#22127 = CARTESIAN_POINT ( 'NONE',  ( 36.36258059203031934, -13.71368208888610773, 72.86986841596736042 ) ) ;
#22128 = CIRCLE ( 'NONE', #8980, 1.000000000000000888 ) ;
#22129 = FACE_OUTER_BOUND ( 'NONE', #11539, .T. ) ;
#22130 = VECTOR ( 'NONE', #16517, 1000.000000000000000 ) ;
#22131 = CIRCLE ( 'NONE', #11036, 0.7106531558045068309 ) ;
#22132 = LINE ( 'NONE', #12366, #21914 ) ;
#22133 = CARTESIAN_POINT ( 'NONE',  ( 45.81606138205700063, 44.92314894770294131, 80.37823623207322044 ) ) ;
#22134 = EDGE_CURVE ( 'NONE', #4343, #19498, #13909, .T. ) ;
#22135 =( NAMED_UNIT ( * ) SI_UNIT ( $, .STERADIAN. ) SOLID_ANGLE_UNIT ( ) );
#22136 = DIRECTION ( 'NONE',  ( -1.000000000000000000, 0.000000000000000000, 0.000000000000000000 ) ) ;
#22137 = DIRECTION ( 'NONE',  ( 1.000000000000000000, 0.000000000000000000, 0.000000000000000000 ) ) ;
#22138 = LINE ( 'NONE', #6183, #17239 ) ;
#22139 = CARTESIAN_POINT ( 'NONE',  ( 37.69225076346193504, -23.81368208888610027, 72.33091598616823603 ) ) ;
#22140 = ORIENTED_EDGE ( 'NONE', *, *, #21347, .T. ) ;
#22141 = PLANE ( 'NONE',  #20151 ) ;
#22142 = ADVANCED_FACE ( 'NONE', ( #18038, #8497 ), #8241, .F. ) ;
#22143 = CARTESIAN_POINT ( 'NONE',  ( 45.81606138205700063, 40.34464305740947765, 81.44836866983821722 ) ) ;
#22144 = ORIENTED_EDGE ( 'NONE', *, *, #23041, .T. ) ;
#22145 = ORIENTED_EDGE ( 'NONE', *, *, #22134, .T. ) ;
#22146 = CARTESIAN_POINT ( 'NONE',  ( 40.33642880535521869, -25.30384086642191477, 69.98269868914864844 ) ) ;
#22147 = VECTOR ( 'NONE', #11165, 1000.000000000000000 ) ;
#22148 = CARTESIAN_POINT ( 'NONE',  ( 39.64521430340304420, 1.186317911113898838, 69.45876917294178554 ) ) ;
#22149 = CARTESIAN_POINT ( 'NONE',  ( 35.64099152588522657, -1.357181138186998925, 79.30501292737000085 ) ) ;
#22150 = VECTOR ( 'NONE', #354, 1000.000000000000000 ) ;
#22151 = CARTESIAN_POINT ( 'NONE',  ( 45.81606138205707168, -36.80651332587431313, 65.82119181171029254 ) ) ;
#22152 = VERTEX_POINT ( 'NONE', #22267 ) ;
#22153 = CARTESIAN_POINT ( 'NONE',  ( 37.31606138205700063, 42.19123852234596939, 66.30501292736988717 ) ) ;
#22154 = LINE ( 'NONE', #20227, #7985 ) ;
#22155 = CARTESIAN_POINT ( 'NONE',  ( 38.37017380507018771, -3.603840866421911038, 69.04448340153881247 ) ) ;
#22156 = VECTOR ( 'NONE', #5347, 1000.000000000000000 ) ;
#22157 = EDGE_CURVE ( 'NONE', #15261, #14953, #7389, .T. ) ;
#22158 = PLANE ( 'NONE',  #17710 ) ;
#22159 = CARTESIAN_POINT ( 'NONE',  ( 36.31606138205700063, 42.19123852234599781, 75.30501292736987295 ) ) ;
#22160 = CARTESIAN_POINT ( 'NONE',  ( 38.37017380507020192, -10.01368208888611022, 73.11602215082118050 ) ) ;
#22161 = PLANE ( 'NONE',  #213 ) ;
#22162 = EDGE_CURVE ( 'NONE', #11694, #12986, #14288, .T. ) ;
#22163 = CARTESIAN_POINT ( 'NONE',  ( 36.68196826583682935, -25.61368208888610454, 71.96809898377887293 ) ) ;
#22164 = EDGE_CURVE ( 'NONE', #19306, #14769, #11995, .T. ) ;
#22165 = AXIS2_PLACEMENT_3D ( 'NONE', #15061, #14941, #22669 ) ;
#22166 = EDGE_CURVE ( 'NONE', #2190, #18244, #12240, .T. ) ;
#22167 = EDGE_CURVE ( 'NONE', #2274, #1644, #22138, .T. ) ;
#22168 = CIRCLE ( 'NONE', #5713, 1.750000000000001554 ) ;
#22169 = LINE ( 'NONE', #2449, #2753 ) ;
#22170 = CARTESIAN_POINT ( 'NONE',  ( 43.31606138205700063, -11.18542543036241632, 17.47151328161626793 ) ) ;
#22171 = AXIS2_PLACEMENT_3D ( 'NONE', #4901, #20489, #9041 ) ;
#22172 = CARTESIAN_POINT ( 'NONE',  ( 38.93987200065210175, -22.80384086642191122, 72.33091598616826445 ) ) ;
#22173 = CARTESIAN_POINT ( 'NONE',  ( 38.93415946300897446, -14.11368208888610631, 73.09843995877329803 ) ) ;
#22174 = DIRECTION ( 'NONE',  ( 2.690219486203388234E-15, -0.8967398287344627850, -0.4425581086832399147 ) ) ;
#22175 = EDGE_CURVE ( 'NONE', #16802, #6235, #4500, .T. ) ;
#22176 = EDGE_CURVE ( 'NONE', #2388, #6126, #23688, .T. ) ;
#22177 = CARTESIAN_POINT ( 'NONE',  ( 36.68196826583682935, -10.00384086642191406, 70.79240656858108593 ) ) ;
#22178 = FACE_OUTER_BOUND ( 'NONE', #4077, .T. ) ;
#22179 = CARTESIAN_POINT ( 'NONE',  ( 39.29254315202756231, -4.813682088886099386, 69.94417936956673998 ) ) ;
#22180 = ORIENTED_EDGE ( 'NONE', *, *, #17059, .T. ) ;
#22181 = CARTESIAN_POINT ( 'NONE',  ( 39.02088643472237095, -14.91368208888609992, 69.02690120949091579 ) ) ;
#22182 = EDGE_LOOP ( 'NONE', ( #12386, #15251, #9726, #18392 ) ) ;
#22183 = CARTESIAN_POINT ( 'NONE',  ( 46.81606138205702194, -20.92507021039837767, 32.39841118875936132 ) ) ;
#22184 = CARTESIAN_POINT ( 'NONE',  ( 44.31606138205700063, -20.88462213365835041, 44.49284693532412405 ) ) ;
#22185 = CARTESIAN_POINT ( 'NONE',  ( 37.60469502381300799, -16.40384086642191264, 72.26730301774234988 ) ) ;
#22186 = VECTOR ( 'NONE', #7230, 1000.000000000000114 ) ;
#22187 = ORIENTED_EDGE ( 'NONE', *, *, #18261, .T. ) ;
#22188 = ADVANCED_FACE ( 'NONE', ( #10430 ), #2549, .F. ) ;
#22189 = ORIENTED_EDGE ( 'NONE', *, *, #17616, .F. ) ;
#22190 = CARTESIAN_POINT ( 'NONE',  ( 35.64099152588522657, -8.607181138186998481, 78.30501292736998664 ) ) ;
#22191 = CARTESIAN_POINT ( 'NONE',  ( 33.31606138205700773, -30.89740888249930961, 1.247106086993583718 ) ) ;
#22192 = CARTESIAN_POINT ( 'NONE',  ( 36.36258059203030513, -21.90384086642191619, 69.89063713639259845 ) ) ;
#22193 = CARTESIAN_POINT ( 'NONE',  ( 32.82453668393288382, -33.17626737717533558, 59.69730689378931032 ) ) ;
#22194 = CARTESIAN_POINT ( 'NONE',  ( 39.82603832034400426, -24.31368208888611093, 72.40698646996131060 ) ) ;
#22195 = LINE ( 'NONE', #17839, #7318 ) ;
#22196 = ORIENTED_EDGE ( 'NONE', *, *, #4054, .F. ) ;
#22197 = VECTOR ( 'NONE', #11417, 1000.000000000000114 ) ;
#22198 = ORIENTED_EDGE ( 'NONE', *, *, #19821, .T. ) ;
#22199 = CARTESIAN_POINT ( 'NONE',  ( 31.81606138205700418, 41.44123852234595518, 61.30501292736988006 ) ) ;
#22200 = DIRECTION ( 'NONE',  ( 0.000000000000000000, 0.8191520442889929088, 0.5735764363510447161 ) ) ;
#22201 = CARTESIAN_POINT ( 'NONE',  ( 37.80618814713138676, -17.70384086642190979, 69.62690120949091011 ) ) ;
#22202 = CARTESIAN_POINT ( 'NONE',  ( 0.000000000000000000, 0.000000000000000000, 0.000000000000000000 ) ) ;
#22203 = PLANE ( 'NONE',  #518 ) ;
#22204 = AXIS2_PLACEMENT_3D ( 'NONE', #5666, #5930, #1916 ) ;
#22205 = DIRECTION ( 'NONE',  ( 0.000000000000000000, -1.000000000000000000, 2.999999999999999839E-15 ) ) ;
#22206 = CARTESIAN_POINT ( 'NONE',  ( 40.31606138205701484, -20.93502329652820038, 27.89939821807130826 ) ) ;
#22207 = CARTESIAN_POINT ( 'NONE',  ( 37.38336156205273397, -1.903840866421910638, 70.63227792289248441 ) ) ;
#22208 = VECTOR ( 'NONE', #20537, 1000.000000000000000 ) ;
#22209 = LINE ( 'NONE', #17977, #5755 ) ;
#22210 = ORIENTED_EDGE ( 'NONE', *, *, #13250, .T. ) ;
#22211 = FACE_OUTER_BOUND ( 'NONE', #14132, .T. ) ;
#22212 = ORIENTED_EDGE ( 'NONE', *, *, #21334, .T. ) ;
#22213 = ORIENTED_EDGE ( 'NONE', *, *, #19323, .F. ) ;
#22214 = CARTESIAN_POINT ( 'NONE',  ( 36.81606138205700063, 8.191238522346989015, 65.30501292736998664 ) ) ;
#22216 = EDGE_CURVE ( 'NONE', #12889, #4199, #18413, .T. ) ;
#22215 = DIRECTION ( 'NONE',  ( 0.000000000000000000, 1.000000000000000000, 0.000000000000000000 ) ) ;
#22217 = VECTOR ( 'NONE', #179, 1000.000000000000000 ) ;
#22218 = CARTESIAN_POINT ( 'NONE',  ( 37.31647492878122563, -7.313682088886101162, 70.72433947564853440 ) ) ;
#22219 = CARTESIAN_POINT ( 'NONE',  ( 38.63098279924288647, -4.913682088886102584, 70.22690120949091863 ) ) ;
#22220 = VERTEX_POINT ( 'NONE', #19048 ) ;
#22221 = PRODUCT_RELATED_PRODUCT_CATEGORY ( 'part', '', ( #19375 ) ) ;
#22222 = ORIENTED_EDGE ( 'NONE', *, *, #8040, .F. ) ;
#22223 = CARTESIAN_POINT ( 'NONE',  ( 33.42374909935192306, 3.629904212211158221, 6.320127632620215152 ) ) ;
#22224 = CARTESIAN_POINT ( 'NONE',  ( 34.56606138205700773, 42.19123852234599781, 75.30501292736987295 ) ) ;
#22225 = ORIENTED_EDGE ( 'NONE', *, *, #23724, .F. ) ;
#22226 =( NAMED_UNIT ( * ) PLANE_ANGLE_UNIT ( ) SI_UNIT ( $, .RADIAN. ) );
#22227 = VECTOR ( 'NONE', #9820, 1000.000000000000000 ) ;
#22228 = CARTESIAN_POINT ( 'NONE',  ( 39.75915168707251723, -8.903840866421916189, 72.49904802271740323 ) ) ;
#22229 = DIRECTION ( 'NONE',  ( 0.000000000000000000, -0.7540134720837687876, -0.6568589528324780824 ) ) ;
#22230 = EDGE_LOOP ( 'NONE', ( #7268, #9889 ) ) ;
#22231 = VERTEX_POINT ( 'NONE', #1001 ) ;
#22232 = ORIENTED_EDGE ( 'NONE', *, *, #12234, .T. ) ;
#22233 = CARTESIAN_POINT ( 'NONE',  ( 42.56606138205700063, 2.740850673309605412, 6.112030963703427133 ) ) ;
#22234 = AXIS2_PLACEMENT_3D ( 'NONE', #9186, #11107, #22689 ) ;
#22235 = CARTESIAN_POINT ( 'NONE',  ( 38.26194895904383486, -9.013682088886101340, 69.64448340153879258 ) ) ;
#22236 = PLANE ( 'NONE',  #17199 ) ;
#22237 = DIRECTION ( 'NONE',  ( 0.000000000000000000, -1.000000000000000000, 0.000000000000000000 ) ) ;
#22238 = AXIS2_PLACEMENT_3D ( 'NONE', #337, #4101, #8219 ) ;
#22239 = EDGE_LOOP ( 'NONE', ( #1516, #17755, #15439, #2033 ) ) ;
#22240 = DIRECTION ( 'NONE',  ( -0.000000000000000000, -3.469446951953613400E-15, -1.000000000000000000 ) ) ;
#22241 = DIRECTION ( 'NONE',  ( 0.000000000000000000, -3.491481338843134933E-15, -1.000000000000000000 ) ) ;
#22242 = CARTESIAN_POINT ( 'NONE',  ( 43.31606138205700063, -27.66931681479738003, 59.51410614687260647 ) ) ;
#22243 = DIRECTION ( 'NONE',  ( 1.000000000000000000, -5.352861011585579840E-16, 1.605858303475673768E-30 ) ) ;
#22244 = EDGE_LOOP ( 'NONE', ( #19416, #7655, #12692, #24981 ) ) ;
#22245 = EDGE_LOOP ( 'NONE', ( #992, #224, #9243, #23649 ) ) ;
#22247 = ADVANCED_FACE ( 'NONE', ( #14658 ), #20850, .T. ) ;
#22246 = DIRECTION ( 'NONE',  ( -1.000000000000000000, -2.065146995210479765E-16, 1.734723475976814737E-16 ) ) ;
#22248 = CARTESIAN_POINT ( 'NONE',  ( 39.73277004305198545, -28.21368208888611306, 73.23812341099225875 ) ) ;
#22249 = EDGE_CURVE ( 'NONE', #25460, #17088, #14540, .T. ) ;
#22251 = AXIS2_PLACEMENT_3D ( 'NONE', #22530, #22791, #2811 ) ;
#22250 = CARTESIAN_POINT ( 'NONE',  ( 38.93987200065208754, -20.81368208888610027, 70.42958956619168021 ) ) ;
#22252 = ORIENTED_EDGE ( 'NONE', *, *, #6170, .T. ) ;
#22253 = ORIENTED_EDGE ( 'NONE', *, *, #4052, .F. ) ;
#22254 = LINE ( 'NONE', #14273, #5429 ) ;
#22255 = CARTESIAN_POINT ( 'NONE',  ( 36.64852494920107517, -11.41368208888610525, 70.89533451361947414 ) ) ;
#22256 = CARTESIAN_POINT ( 'NONE',  ( 37.25260217561390874, -2.003840866421909617, 70.97781676520604321 ) ) ;
#22257 = VECTOR ( 'NONE', #14108, 1000.000000000000000 ) ;
#22258 = DIRECTION ( 'NONE',  ( 0.000000000000000000, 1.000000000000000000, -2.999999999999999839E-15 ) ) ;
#22259 = CARTESIAN_POINT ( 'NONE',  ( 36.36258059203031934, -11.71368208888610951, 72.86986841596736042 ) ) ;
#22260 = CARTESIAN_POINT ( 'NONE',  ( 46.81606138205695800, -0.7562224151693112129, -1.633662118351544734 ) ) ;
#22261 = CARTESIAN_POINT ( 'NONE',  ( 34.06606138205700773, -37.53049398575952722, 70.06662099985001646 ) ) ;
#22262 = ADVANCED_FACE ( 'NONE', ( #8625 ), #16989, .T. ) ;
#22263 = FACE_OUTER_BOUND ( 'NONE', #3076, .T. ) ;
#22264 = DIRECTION ( 'NONE',  ( 0.000000000000000000, -1.000000000000000000, 2.999999999999999839E-15 ) ) ;
#22265 = FACE_OUTER_BOUND ( 'NONE', #20666, .T. ) ;
#22266 = AXIS2_PLACEMENT_3D ( 'NONE', #9881, #6260, #23773 ) ;
#22267 = CARTESIAN_POINT ( 'NONE',  ( 31.81606138205700418, 44.92314894770293421, 79.37823623207320622 ) ) ;
#22268 = ORIENTED_EDGE ( 'NONE', *, *, #4558, .T. ) ;
#22269 = FACE_OUTER_BOUND ( 'NONE', #718, .T. ) ;
#22270 = AXIS2_PLACEMENT_3D ( 'NONE', #11761, #23455, #7497 ) ;
#22271 = CARTESIAN_POINT ( 'NONE',  ( 40.64099152588523367, -8.607181138186998481, 79.30501292737000085 ) ) ;
#22272 = ORIENTED_EDGE ( 'NONE', *, *, #13214, .T. ) ;
#22273 = ORIENTED_EDGE ( 'NONE', *, *, #15156, .F. ) ;
#22274 = CARTESIAN_POINT ( 'NONE',  ( 38.37017380507018771, -23.60384086642191903, 69.04448340153878405 ) ) ;
#22275 = CARTESIAN_POINT ( 'NONE',  ( 37.33957961208646736, -25.81368208888610738, 72.81632618279320468 ) ) ;
#22276 = DIRECTION ( 'NONE',  ( -1.000000000000000000, -2.999999999999999839E-15, 0.000000000000000000 ) ) ;
#22277 = CARTESIAN_POINT ( 'NONE',  ( 41.96606138205694947, 5.208890205473748480, 5.429380561359602453 ) ) ;
#22278 =( LENGTH_UNIT ( ) NAMED_UNIT ( * ) SI_UNIT ( .MILLI., .METRE. ) );
#22279 = VERTEX_POINT ( 'NONE', #22399 ) ;
#22280 = DIRECTION ( 'NONE',  ( -1.000000000000000000, -1.734723475976804876E-16, 1.734723475976814737E-16 ) ) ;
#22281 = DIRECTION ( 'NONE',  ( -3.491481338843135327E-15, 1.000000000000000000, -2.999999999999999050E-15 ) ) ;
#22282 = CARTESIAN_POINT ( 'NONE',  ( 37.50301148336529167, -25.11368208888610454, 69.06206559358663810 ) ) ;
#22283 = AXIS2_PLACEMENT_3D ( 'NONE', #15692, #21624, #222 ) ;
#22284 = LINE ( 'NONE', #12260, #17278 ) ;
#22285 = CARTESIAN_POINT ( 'NONE',  ( 33.31606138205700773, -19.47805968271055477, 24.94720442500192448 ) ) ;
#22286 = CARTESIAN_POINT ( 'NONE',  ( 40.14115730948191185, -6.513682088886103116, 71.32335560751961623 ) ) ;
#22287 = DIRECTION ( 'NONE',  ( 3.717264591378870232E-16, 3.130104260698260371E-15, 1.000000000000000000 ) ) ;
#22288 = ADVANCED_FACE ( 'NONE', ( #22522 ), #16593, .T. ) ;
#22289 = VECTOR ( 'NONE', #719, 1000.000000000000000 ) ;
#22290 = CARTESIAN_POINT ( 'NONE',  ( 37.69796330110504101, -23.11368208888609743, 69.66206559358661821 ) ) ;
#22291 = CARTESIAN_POINT ( 'NONE',  ( 45.81606138205700063, -33.05876147765410167, 70.30501292737000085 ) ) ;
#22292 = CARTESIAN_POINT ( 'NONE',  ( 30.81606138205700418, 39.39281886181299797, 81.75501292736984738 ) ) ;
#22293 = CARTESIAN_POINT ( 'NONE',  ( 38.63098279924290068, -22.70384086642191335, 72.53360434286904024 ) ) ;
#22294 = CARTESIAN_POINT ( 'NONE',  ( 38.93415946300897446, -10.11368208888610987, 73.09843995877331224 ) ) ;
#22295 = LINE ( 'NONE', #8664, #13953 ) ;
#22296 = CIRCLE ( 'NONE', #25148, 1.499999999999999778 ) ;
#22297 = EDGE_LOOP ( 'NONE', ( #24450, #10263, #14452, #21933 ) ) ;
#22298 = VECTOR ( 'NONE', #858, 1000.000000000000000 ) ;
#22299 = CARTESIAN_POINT ( 'NONE',  ( 38.82593461698265003, -8.703840866421909794, 73.13360434286904876 ) ) ;
#22300 = ADVANCED_FACE ( 'NONE', ( #7065 ), #18786, .F. ) ;
#22301 = DIRECTION ( 'NONE',  ( -1.734723475976814737E-16, 1.000000000000000000, -3.491481338843135327E-15 ) ) ;
#22302 = APPLICATION_CONTEXT ( 'automotive_design' ) ;
#22303 = ADVANCED_FACE ( 'NONE', ( #12624 ), #4876, .F. ) ;
#22304 = CIRCLE ( 'NONE', #11201, 1.500000000000001332 ) ;
#22305 = CARTESIAN_POINT ( 'NONE',  ( 36.80608444377001121, -3.313682088886100718, 70.35351908239860563 ) ) ;
#22306 = VERTEX_POINT ( 'NONE', #24440 ) ;
#22307 = CARTESIAN_POINT ( 'NONE',  ( 38.26194895904383486, -13.01368208888610312, 69.04448340153878405 ) ) ;
#22308 = VERTEX_POINT ( 'NONE', #14915 ) ;
#22309 = CARTESIAN_POINT ( 'NONE',  ( 36.31606138205700063, 37.94123852234599781, 75.30501292736988717 ) ) ;
#22310 = EDGE_CURVE ( 'NONE', #21429, #4268, #5002, .T. ) ;
#22311 = CARTESIAN_POINT ( 'NONE',  ( 35.81606138205700063, -31.05876147765399864, 75.30501292737010033 ) ) ;
#22312 = CARTESIAN_POINT ( 'NONE',  ( 39.37952058850012804, -9.003840866421910505, 71.78268878715392987 ) ) ;
#22313 = EDGE_CURVE ( 'NONE', #15455, #23735, #24556, .T. ) ;
#22314 = EDGE_CURVE ( 'NONE', #17064, #13535, #2926, .T. ) ;
#22315 = ORIENTED_EDGE ( 'NONE', *, *, #9784, .T. ) ;
#22316 = ORIENTED_EDGE ( 'NONE', *, *, #14678, .T. ) ;
#22317 = LINE ( 'NONE', #4791, #20360 ) ;
#22318 = DIRECTION ( 'NONE',  ( -1.000000000000000000, -0.000000000000000000, -0.000000000000000000 ) ) ;
#22319 = CARTESIAN_POINT ( 'NONE',  ( 39.12911128074872380, -23.50384086642191050, 69.06206559358665231 ) ) ;
#22320 = CYLINDRICAL_SURFACE ( 'NONE', #12839, 1.000000000000000888 ) ;
#22321 = CARTESIAN_POINT ( 'NONE',  ( 40.77203464402485622, 1.486317911113896661, 71.32335560751961623 ) ) ;
#22322 = CARTESIAN_POINT ( 'NONE',  ( 38.31606138205700063, -29.30876147765400930, 71.30501292737010033 ) ) ;
#22323 = ADVANCED_FACE ( 'NONE', ( #22778 ), #16858, .T. ) ;
#22324 = CARTESIAN_POINT ( 'NONE',  ( 33.56606138205700773, 41.44123852234599070, 73.55501292736987295 ) ) ;
#22325 = EDGE_CURVE ( 'NONE', #24574, #7575, #774, .T. ) ;
#22326 = AXIS2_PLACEMENT_3D ( 'NONE', #3538, #1852, #11414 ) ;
#22327 = VERTEX_POINT ( 'NONE', #6938 ) ;
#22328 = DIRECTION ( 'NONE',  ( -1.734723475976814737E-16, 1.000000000000000000, -3.491481338843135327E-15 ) ) ;
#22329 = PLANE ( 'NONE',  #17583 ) ;
#22330 = VECTOR ( 'NONE', #17104, 1000.000000000000000 ) ;
#22331 = CARTESIAN_POINT ( 'NONE',  ( 39.98359781491296161, -15.20384086642191157, 70.89533451361945993 ) ) ;
#22332 = CARTESIAN_POINT ( 'NONE',  ( 0.000000000000000000, 0.000000000000000000, 0.000000000000000000 ) ) ;
#22333 = DIRECTION ( 'NONE',  ( -1.000000000000000000, 0.000000000000000000, 0.000000000000000000 ) ) ;
#22334 = LINE ( 'NONE', #24246, #11906 ) ;
#22335 = ADVANCED_FACE ( 'NONE', ( #22651 ), #12873, .T. ) ;
#22336 = CARTESIAN_POINT ( 'NONE',  ( 32.81606138205700773, -37.81581049437288300, 70.47722359350072452 ) ) ;
#22337 = CARTESIAN_POINT ( 'NONE',  ( 39.51027997493896748, 0.8961591335780900724, 71.43714994484035685 ) ) ;
#22338 = CARTESIAN_POINT ( 'NONE',  ( 38.05466885408097255, -22.20914808198024559, 75.80498909504116511 ) ) ;
#22339 = ORIENTED_EDGE ( 'NONE', *, *, #9290, .F. ) ;
#22340 = AXIS2_PLACEMENT_3D ( 'NONE', #19122, #23345, #23098 ) ;
#22341 = CARTESIAN_POINT ( 'NONE',  ( 39.38009889167650357, -24.21368208888610596, 72.75271321436730432 ) ) ;
#22342 = ORIENTED_EDGE ( 'NONE', *, *, #4114, .T. ) ;
#22343 = ORIENTED_EDGE ( 'NONE', *, *, #10182, .F. ) ;
#22344 = DIRECTION ( 'NONE',  ( 1.000000000000000000, -0.000000000000000000, -0.000000000000000000 ) ) ;
#22345 = VECTOR ( 'NONE', #1187, 1000.000000000000000 ) ;
#22346 = CYLINDRICAL_SURFACE ( 'NONE', #11297, 0.5000000000000004441 ) ;
#22347 = CARTESIAN_POINT ( 'NONE',  ( 39.37952058850012804, -2.613682088886102761, 70.97781676520601479 ) ) ;
#22348 = CARTESIAN_POINT ( 'NONE',  ( 37.21915885897815457, -1.413682088886099253, 71.08074471024443142 ) ) ;
#22349 = ORIENTED_EDGE ( 'NONE', *, *, #3567, .F. ) ;
#22350 = ORIENTED_EDGE ( 'NONE', *, *, #24060, .T. ) ;
#22351 = DIRECTION ( 'NONE',  ( 0.000000000000000000, 1.000000000000000000, -2.999999999999999839E-15 ) ) ;
#22352 = AXIS2_PLACEMENT_3D ( 'NONE', #20545, #8958, #6886 ) ;
#22353 = CARTESIAN_POINT ( 'NONE',  ( 32.81606138205700773, 41.44123852234595518, 61.30501292736988006 ) ) ;
#22354 = VERTEX_POINT ( 'NONE', #18920 ) ;
#22355 = CARTESIAN_POINT ( 'NONE',  ( 39.95015449827720744, -13.00384086642191228, 71.96809898377887293 ) ) ;
#22356 = PLANE ( 'NONE',  #14161 ) ;
#22357 = VECTOR ( 'NONE', #11154, 1000.000000000000227 ) ;
#22358 = CARTESIAN_POINT ( 'NONE',  ( 40.81606138205700773, 41.44123852234599781, 75.30501292736988717 ) ) ;
#22359 = EDGE_LOOP ( 'NONE', ( #4517, #8374, #14616, #25039 ) ) ;
#22360 = ORIENTED_EDGE ( 'NONE', *, *, #16508, .F. ) ;
#22361 = ORIENTED_EDGE ( 'NONE', *, *, #15238, .F. ) ;
#22362 = FACE_OUTER_BOUND ( 'NONE', #12197, .T. ) ;
#22363 = STYLED_ITEM ( 'NONE', ( #11035 ), #6130 ) ;
#22364 = CARTESIAN_POINT ( 'NONE',  ( 36.87297107704153376, -9.713682088886107735, 72.49904802271743165 ) ) ;
#22365 = LINE ( 'NONE', #12970, #11448 ) ;
#22366 = VECTOR ( 'NONE', #13527, 1000.000000000000227 ) ;
#22367 = DIRECTION ( 'NONE',  ( 1.000000000000000000, 8.911169920151748851E-16, 3.114923731923493702E-16 ) ) ;
#22368 = DIRECTION ( 'NONE',  ( 0.000000000000000000, 1.000000000000000000, -2.999999999999999839E-15 ) ) ;
#22369 = EDGE_CURVE ( 'NONE', #17597, #13983, #9143, .T. ) ;
#22370 = AXIS2_PLACEMENT_3D ( 'NONE', #12388, #9943, #6200 ) ;
#22371 = DIRECTION ( 'NONE',  ( 1.000000000000000000, 0.000000000000000000, 0.000000000000000000 ) ) ;
#22372 = CARTESIAN_POINT ( 'NONE',  ( 36.52583090115293629, -6.250151542416438666, 82.75087430736850536 ) ) ;
#22373 = AXIS2_PLACEMENT_3D ( 'NONE', #11991, #18976, #11124 ) ;
#22374 = CARTESIAN_POINT ( 'NONE',  ( 40.31606138205701484, -20.93502329652820038, 27.89939821807130826 ) ) ;
#22375 = ORIENTED_EDGE ( 'NONE', *, *, #20629, .F. ) ;
#22376 = ORIENTED_EDGE ( 'NONE', *, *, #20422, .T. ) ;
#22377 = LINE ( 'NONE', #6656, #19831 ) ;
#22378 = CARTESIAN_POINT ( 'NONE',  ( 40.55423172469004811, -26.41368208888610880, 72.05058123536539938 ) ) ;
#22379 = STYLED_ITEM ( 'NONE', ( #3928 ), #24269 ) ;
#22380 = CARTESIAN_POINT ( 'NONE',  ( 37.12184278917507640, -25.51368208888609956, 71.43714994484032843 ) ) ;
#22381 = EDGE_LOOP ( 'NONE', ( #21768, #3820, #22343, #958 ) ) ;
#22382 = VERTEX_POINT ( 'NONE', #7201 ) ;
#22383 = DIRECTION ( 'NONE',  ( 1.000000000000000000, 0.000000000000000000, 0.000000000000000000 ) ) ;
#22384 = CARTESIAN_POINT ( 'NONE',  ( 37.25202387243752611, -5.213682088886100630, 70.00779233799264034 ) ) ;
#22385 = CARTESIAN_POINT ( 'NONE',  ( 37.89291511884479036, -0.5038408664219118371, 72.49843995877331793 ) ) ;
#22386 = VECTOR ( 'NONE', #21839, 1000.000000000000000 ) ;
#22387 = CARTESIAN_POINT ( 'NONE',  ( 33.31606138205700773, -22.22127907754180853, 85.30501292736998664 ) ) ;
#22388 = CIRCLE ( 'NONE', #22788, 0.7500000000000006661 ) ;
#22389 = CARTESIAN_POINT ( 'NONE',  ( 35.86008812008917346, -7.513682088886104893, 71.43714994484035685 ) ) ;
#22390 = CARTESIAN_POINT ( 'NONE',  ( 36.31606138205700063, -26.06829118875199569, 75.80501292736998664 ) ) ;
#22391 = DIRECTION ( 'NONE',  ( 1.734723475976805122E-15, 2.999999999999999839E-15, 1.000000000000000000 ) ) ;
#22392 = DIRECTION ( 'NONE',  ( -1.000000000000000000, -3.091505625455828697E-15, -4.515976121274772923E-17 ) ) ;
#22393 = ADVANCED_FACE ( 'NONE', ( #15044 ), #5263, .T. ) ;
#22394 = LINE ( 'NONE', #22133, #1730 ) ;
#22395 = EDGE_CURVE ( 'NONE', #18393, #2190, #13256, .T. ) ;
#22396 = PRODUCT_DEFINITION_FORMATION_WITH_SPECIFIED_SOURCE ( 'ANY', '', #7876, .NOT_KNOWN. ) ;
#22397 = DIRECTION ( 'NONE',  ( 0.000000000000000000, 1.000000000000000000, -2.999999999999999839E-15 ) ) ;
#22398 = CIRCLE ( 'NONE', #20751, 0.2000000000000057288 ) ;
#22399 = CARTESIAN_POINT ( 'NONE',  ( 33.31606138205700063, -13.43064139120330758, 11.56373968489310755 ) ) ;
#22400 = VERTEX_POINT ( 'NONE', #25196 ) ;
#22401 = CARTESIAN_POINT ( 'NONE',  ( 38.58006293444520196, -22.20810519139199002, 75.30498852987368252 ) ) ;
#22402 = CARTESIAN_POINT ( 'NONE',  ( 33.31606138205700773, -11.22674583108233115, 81.40610939240433197 ) ) ;
#22403 = VERTEX_POINT ( 'NONE', #11837 ) ;
#22404 = EDGE_LOOP ( 'NONE', ( #14774, #11415, #14218, #17193 ) ) ;
#22405 = CARTESIAN_POINT ( 'NONE',  ( 39.02088643472237806, -16.70384086642191690, 73.73360434286898624 ) ) ;
#22406 = EDGE_CURVE ( 'NONE', #16742, #3435, #15990, .T. ) ;
#22407 = CARTESIAN_POINT ( 'NONE',  ( 39.29254315202756231, -22.81368208888610027, 69.94417936956672577 ) ) ;
#22408 = CARTESIAN_POINT ( 'NONE',  ( 32.81606138205700773, 36.92314894770294131, 81.17823623207323180 ) ) ;
#22409 = DIRECTION ( 'NONE',  ( 0.000000000000000000, 1.000000000000000000, 0.000000000000000000 ) ) ;
#22410 = VERTEX_POINT ( 'NONE', #1392 ) ;
#22411 = CARTESIAN_POINT ( 'NONE',  ( 36.31606138205702194, -19.58709462196291184, 24.03834292329984379 ) ) ;
#22412 = CARTESIAN_POINT ( 'NONE',  ( 30.81606138205700418, 44.92314894770294131, 81.17823623207321759 ) ) ;
#22413 = CARTESIAN_POINT ( 'NONE',  ( 39.73277004305197124, 0.5961591335780883627, 69.52238214136770011 ) ) ;
#22414 = VERTEX_POINT ( 'NONE', #11331 ) ;
#22415 = VECTOR ( 'NONE', #13805, 1000.000000000000000 ) ;
#22416 = DIRECTION ( 'NONE',  ( 0.000000000000000000, 0.3299742535180974490, -0.9439899321577398528 ) ) ;
#22417 = CARTESIAN_POINT ( 'NONE',  ( 40.31606138205700063, 5.691238522346998785, 68.80501292736998664 ) ) ;
#22418 = CARTESIAN_POINT ( 'NONE',  ( 39.38009889167650357, 1.786317911113891821, 72.75271321436734695 ) ) ;
#22419 = DIRECTION ( 'NONE',  ( -1.000000000000000000, 0.000000000000000000, 0.000000000000000000 ) ) ;
#22420 = CARTESIAN_POINT ( 'NONE',  ( 38.93415946300898867, -18.11368208888610809, 73.09843995877329803 ) ) ;
#22421 = LINE ( 'NONE', #2698, #12722 ) ;
#22422 = CARTESIAN_POINT ( 'NONE',  ( 35.31606138205687273, 43.19123852234596939, 65.30501292736988717 ) ) ;
#22423 = CARTESIAN_POINT ( 'NONE',  ( 37.21915885897815457, -24.20384086642190979, 71.67976084211551324 ) ) ;
#22424 = CARTESIAN_POINT ( 'NONE',  ( 39.75915168707250302, -6.713682088886099741, 70.26145752964252722 ) ) ;
#22425 = VERTEX_POINT ( 'NONE', #13386 ) ;
#22426 = DIRECTION ( 'NONE',  ( -1.000000000000000000, -2.999999999999999839E-15, 0.000000000000000000 ) ) ;
#22427 = ORIENTED_EDGE ( 'NONE', *, *, #14937, .T. ) ;
#22428 = VECTOR ( 'NONE', #373, 1000.000000000000000 ) ;
#22429 = CARTESIAN_POINT ( 'NONE',  ( 36.49096545463212493, -4.103840866421911038, 71.32335560751963044 ) ) ;
#22430 = DIRECTION ( 'NONE',  ( -1.445602896647339656E-16, 0.8212051873014208914, 0.5706330172266919076 ) ) ;
#22431 = EDGE_CURVE ( 'NONE', #14130, #17105, #15300, .T. ) ;
#22432 = CARTESIAN_POINT ( 'NONE',  ( 36.87297107704152666, -5.713682088886105959, 72.49904802271743165 ) ) ;
#22433 = VERTEX_POINT ( 'NONE', #13631 ) ;
#22434 = CARTESIAN_POINT ( 'NONE',  ( 38.37017380507020192, -14.01368208888610845, 73.71602215082113219 ) ) ;
#22435 = ORIENTED_EDGE ( 'NONE', *, *, #19644, .T. ) ;
#22436 = LINE ( 'NONE', #24862, #16883 ) ;
#22437 = CARTESIAN_POINT ( 'NONE',  ( 17.31606138205699708, 34.87886987267149408, 78.19668729537065133 ) ) ;
#22438 = CARTESIAN_POINT ( 'NONE',  ( 38.93987200065210175, -14.80384086642191122, 72.33091598616826445 ) ) ;
#22439 = CARTESIAN_POINT ( 'NONE',  ( 43.81606138205700063, 41.44123852234595518, 61.30501292736988006 ) ) ;
#22440 = EDGE_LOOP ( 'NONE', ( #17713, #20244, #14491, #1007 ) ) ;
#22441 = CARTESIAN_POINT ( 'NONE',  ( 32.81606138205700773, 44.92314894770293421, 79.37823623207320622 ) ) ;
#22442 = CARTESIAN_POINT ( 'NONE',  ( 34.06606138205700773, -40.21665604226827639, 68.80894170722476133 ) ) ;
#22443 = CARTESIAN_POINT ( 'NONE',  ( 40.52078840805429394, -15.00384086642191583, 72.15350918040381600 ) ) ;
#22444 = FACE_OUTER_BOUND ( 'NONE', #2606, .T. ) ;
#22445 = CYLINDRICAL_SURFACE ( 'NONE', #13355, 2.000000000000001776 ) ;
#22446 = CARTESIAN_POINT ( 'NONE',  ( 39.38009889167650357, -22.21368208888610951, 72.75271321436731853 ) ) ;
#22447 = CARTESIAN_POINT ( 'NONE',  ( 44.81606138205700063, -36.10876147765401356, 70.30501292737011454 ) ) ;
#22448 = CARTESIAN_POINT ( 'NONE',  ( 32.81606138205700773, 22.19123852234699967, 69.30501292736994401 ) ) ;
#22449 = EDGE_CURVE ( 'NONE', #6502, #2759, #17119, .T. ) ;
#22450 = ORIENTED_EDGE ( 'NONE', *, *, #9727, .T. ) ;
#22451 = DIRECTION ( 'NONE',  ( 1.000000000000000000, 0.000000000000000000, 0.000000000000000000 ) ) ;
#22452 = EDGE_CURVE ( 'NONE', #22279, #2625, #7323, .T. ) ;
#22453 = CYLINDRICAL_SURFACE ( 'NONE', #23746, 0.5000000000000004441 ) ;
#22454 = CARTESIAN_POINT ( 'NONE',  ( 39.75915168707251723, -12.90384086642191797, 72.49904802271738902 ) ) ;
#22455 = DIRECTION ( 'NONE',  ( 0.000000000000000000, 0.000000000000000000, 1.000000000000000000 ) ) ;
#22456 = CARTESIAN_POINT ( 'NONE',  ( 43.81608638205700146, -3.566646240838321269, 18.16837712155798457 ) ) ;
#22457 = EDGE_CURVE ( 'NONE', #19683, #17745, #21351, .T. ) ;
#22458 = CARTESIAN_POINT ( 'NONE',  ( 38.31606138205700063, -3.742417511052531509, 58.76316301854844681 ) ) ;
#22459 = LINE ( 'NONE', #13288, #3292 ) ;
#22460 = CARTESIAN_POINT ( 'NONE',  ( 40.14115730948191185, -25.10384086642190482, 71.43714994484028580 ) ) ;
#22461 = CARTESIAN_POINT ( 'NONE',  ( 36.99159426505191561, -5.675941582597428869, 82.78927371634733845 ) ) ;
#22462 = ORIENTED_EDGE ( 'NONE', *, *, #23401, .F. ) ;
#22463 = ADVANCED_FACE ( 'NONE', ( #24935 ), #7707, .F. ) ;
#22464 = CARTESIAN_POINT ( 'NONE',  ( 38.26194895904383486, -23.01368208888609956, 69.64448340153877837 ) ) ;
#22465 = ORIENTED_EDGE ( 'NONE', *, *, #2785, .T. ) ;
#22466 = ORIENTED_EDGE ( 'NONE', *, *, #13372, .F. ) ;
#22467 = DIRECTION ( 'NONE',  ( 2.690219486203388234E-15, -0.8967398287344627850, -0.4425581086832399147 ) ) ;
#22468 = B_SPLINE_CURVE_WITH_KNOTS ( 'NONE', 3,
 ( #5090, #19126, #10890, #5344 ),
 .UNSPECIFIED., .F., .F.,
 ( 4, 4 ),
 ( 0.000000000000000000, 1.000000000000000000 ),
 .UNSPECIFIED. ) ;
#22469 = DIRECTION ( 'NONE',  ( 0.000000000000000000, 0.000000000000000000, 1.000000000000000000 ) ) ;
#22470 = CARTESIAN_POINT ( 'NONE',  ( 38.37017380507020192, -2.013682088886102228, 72.51602215082118619 ) ) ;
#22471 = CARTESIAN_POINT ( 'NONE',  ( 38.26194895904383486, -1.013682088886101784, 70.24448340153877268 ) ) ;
#22472 = ORIENTED_EDGE ( 'NONE', *, *, #20599, .T. ) ;
#22473 = VERTEX_POINT ( 'NONE', #17240 ) ;
#22474 = CARTESIAN_POINT ( 'NONE',  ( 44.06606138205700063, 43.35512946304240245, 81.37823623207322044 ) ) ;
#22475 = DIRECTION ( 'NONE',  ( 3.717264591378870232E-16, 2.999999999999999839E-15, 1.000000000000000000 ) ) ;
#22476 = ORIENTED_EDGE ( 'NONE', *, *, #19763, .T. ) ;
#22477 = PLANE ( 'NONE',  #4080 ) ;
#22478 = CARTESIAN_POINT ( 'NONE',  ( 36.49096545463212493, -4.103840866421911038, 71.32335560751963044 ) ) ;
#22479 = FACE_OUTER_BOUND ( 'NONE', #658, .T. ) ;
#22480 = FACE_OUTER_BOUND ( 'NONE', #21682, .T. ) ;
#22481 = VERTEX_POINT ( 'NONE', #1628 ) ;
#22482 = ORIENTED_EDGE ( 'NONE', *, *, #24048, .F. ) ;
#22483 = ADVANCED_FACE ( 'NONE', ( #15551 ), #9273, .F. ) ;
#22484 = ORIENTED_EDGE ( 'NONE', *, *, #25452, .F. ) ;
#22485 = CARTESIAN_POINT ( 'NONE',  ( 33.56606138205700773, 43.19123852234599781, 74.30501292736987295 ) ) ;
#22486 = EDGE_CURVE ( 'NONE', #24557, #7305, #13543, .T. ) ;
#22487 = CARTESIAN_POINT ( 'NONE',  ( 36.87297107704153376, 0.2863179111138939303, 72.49904802271743165 ) ) ;
#22488 = CARTESIAN_POINT ( 'NONE',  ( 38.53272007700518742, 38.69123852234600491, 72.53609335118615320 ) ) ;
#22489 = FACE_OUTER_BOUND ( 'NONE', #530, .T. ) ;
#22490 = EDGE_CURVE ( 'NONE', #10963, #1296, #2420, .T. ) ;
#22491 = EDGE_CURVE ( 'NONE', #10628, #8863, #8214, .T. ) ;
#22492 = CYLINDRICAL_SURFACE ( 'NONE', #15562, 10.50000000000000000 ) ;
#22493 = CARTESIAN_POINT ( 'NONE',  ( 43.81606138205700063, 18.19123852234599426, 73.05501292736995822 ) ) ;
#22494 = DIRECTION ( 'NONE',  ( 0.000000000000000000, -0.1999999999999969580, 0.9797958971132719741 ) ) ;
#22495 = EDGE_CURVE ( 'NONE', #14751, #8838, #22606, .T. ) ;
#22496 = PLANE ( 'NONE',  #19365 ) ;
#22497 = ORIENTED_EDGE ( 'NONE', *, *, #3341, .T. ) ;
#22498 = ORIENTED_EDGE ( 'NONE', *, *, #17489, .T. ) ;
#22499 = DIRECTION ( 'NONE',  ( 1.000000000000000000, 0.000000000000000000, 0.000000000000000000 ) ) ;
#22500 = CARTESIAN_POINT ( 'NONE',  ( 39.73277004305197124, 0.5961591335780883627, 69.52238214136770011 ) ) ;
#22501 = CARTESIAN_POINT ( 'NONE',  ( 35.64099152588522657, 1.142818861812999742, 82.55501292736997243 ) ) ;
#22502 = VECTOR ( 'NONE', #17715, 1000.000000000000000 ) ;
#22503 = AXIS2_PLACEMENT_3D ( 'NONE', #24216, #8794, #2834 ) ;
#22504 = CARTESIAN_POINT ( 'NONE',  ( 39.51027997493896748, -20.51368208888610312, 71.32335560751960202 ) ) ;
#22505 = ORIENTED_EDGE ( 'NONE', *, *, #15561, .T. ) ;
#22506 = ORIENTED_EDGE ( 'NONE', *, *, #12974, .F. ) ;
#22507 = DIRECTION ( 'NONE',  ( 0.000000000000000000, 1.000000000000000000, -2.999999999999999839E-15 ) ) ;
#22508 = CARTESIAN_POINT ( 'NONE',  ( 38.82593461698262871, -0.9136820888861022505, 69.62690120949091011 ) ) ;
#22509 = CARTESIAN_POINT ( 'NONE',  ( 38.73920764526923932, -1.503840866421912725, 70.26206559358664094 ) ) ;
#22510 = CARTESIAN_POINT ( 'NONE',  ( 43.31606138205700063, -10.80800258567212602, 32.62011605800211811 ) ) ;
#22511 = EDGE_CURVE ( 'NONE', #7904, #19498, #25065, .T. ) ;
#22512 = CARTESIAN_POINT ( 'NONE',  ( 36.07789103942398867, -5.413682088886107024, 70.70992431699450265 ) ) ;
#22513 = DIRECTION ( 'NONE',  ( 1.000000000000000000, 0.000000000000000000, 0.000000000000000000 ) ) ;
#22514 = CARTESIAN_POINT ( 'NONE',  ( 44.81606138205700063, 38.19123852234599070, 72.05501292736988717 ) ) ;
#22515 = CARTESIAN_POINT ( 'NONE',  ( 33.56606138205700773, 41.44123852234599781, 74.30501292736987295 ) ) ;
#22516 = CIRCLE ( 'NONE', #3586, 1.500000000000001332 ) ;
#22517 = CARTESIAN_POINT ( 'NONE',  ( 43.81606138205700063, -27.52349462642295208, 56.67559192035834315 ) ) ;
#22518 = VECTOR ( 'NONE', #1682, 1000.000000000000114 ) ;
#22519 = VECTOR ( 'NONE', #15411, 1000.000000000000000 ) ;
#22520 = LINE ( 'NONE', #10803, #9450 ) ;
#22521 = DIRECTION ( 'NONE',  ( 4.584595141645219056E-18, 0.5706330172266919076, -0.8212051873014208914 ) ) ;
#22522 = FACE_OUTER_BOUND ( 'NONE', #6418, .T. ) ;
#22523 = ORIENTED_EDGE ( 'NONE', *, *, #18787, .T. ) ;
#22524 = CARTESIAN_POINT ( 'NONE',  ( 39.53940869104339839, -21.80888753443083772, 75.31325401218029469 ) ) ;
#22525 = LINE ( 'NONE', #16862, #18542 ) ;
#22526 = ORIENTED_EDGE ( 'NONE', *, *, #22645, .F. ) ;
#22527 = ORIENTED_EDGE ( 'NONE', *, *, #11171, .T. ) ;
#22528 = CARTESIAN_POINT ( 'NONE',  ( 36.89935272106205133, -14.40384086642191974, 73.23812341099225875 ) ) ;
#22529 = CARTESIAN_POINT ( 'NONE',  ( 38.26194895904383486, -19.01368208888610312, 69.64448340153877837 ) ) ;
#22530 = CARTESIAN_POINT ( 'NONE',  ( 43.23147868389327897, 41.43850569188389699, 79.37823623207322044 ) ) ;
#22531 = AXIS2_PLACEMENT_3D ( 'NONE', #8347, #596, #20061 ) ;
#22532 = EDGE_CURVE ( 'NONE', #21203, #6883, #4512, .T. ) ;
#22533 = EDGE_CURVE ( 'NONE', #12836, #20252, #3277, .T. ) ;
#22534 = AXIS2_PLACEMENT_3D ( 'NONE', #7022, #19004, #14871 ) ;
#22535 = VECTOR ( 'NONE', #16182, 1000.000000000000000 ) ;
#22536 = LINE ( 'NONE', #4887, #24170 ) ;
#22537 = DIRECTION ( 'NONE',  ( 1.000000000000000000, 0.000000000000000000, 0.000000000000000000 ) ) ;
#22538 = EDGE_LOOP ( 'NONE', ( #12409, #20964, #11717, #12219 ) ) ;
#22539 = CARTESIAN_POINT ( 'NONE',  ( 32.81606138205700773, 35.44123852234597649, 67.80501292736990138 ) ) ;
#22540 = PRODUCT_RELATED_PRODUCT_CATEGORY ( 'part', '', ( #3964 ) ) ;
#22541 = DIRECTION ( 'NONE',  ( 0.9835979625596985576, -0.1803747433772529551, -2.086002012065456372E-15 ) ) ;
#22542 = CARTESIAN_POINT ( 'NONE',  ( 38.26194895904383486, -29.01368208888610312, 69.04448340153878405 ) ) ;
#22543 = ORIENTED_EDGE ( 'NONE', *, *, #22164, .T. ) ;
#22544 = DIRECTION ( 'NONE',  ( 0.000000000000000000, -0.6568589528324746407, 0.7540134720837717852 ) ) ;
#22545 = CYLINDRICAL_SURFACE ( 'NONE', #19031, 1.500000000000001332 ) ;
#22546 = CARTESIAN_POINT ( 'NONE',  ( 39.82603832034400426, -0.3136820888861094336, 72.40698646996135324 ) ) ;
#22547 = DIRECTION ( 'NONE',  ( 1.000000000000000000, 2.751104698760144965E-15, -1.228345504986737969E-16 ) ) ;
#22548 = CARTESIAN_POINT ( 'NONE',  ( 39.95015449827720744, -22.61368208888610809, 70.79240656858105751 ) ) ;
#22549 = DIRECTION ( 'NONE',  ( 0.000000000000000000, 0.000000000000000000, -1.000000000000000000 ) ) ;
#22550 = EDGE_CURVE ( 'NONE', #13391, #2309, #21352, .T. ) ;
#22551 = CARTESIAN_POINT ( 'NONE',  ( 40.31606138205700773, -11.51539968388051705, 18.41550321377400934 ) ) ;
#22552 = CARTESIAN_POINT ( 'NONE',  ( 37.89291511884479036, -20.50384086642191406, 72.49843995877330372 ) ) ;
#22553 = CARTESIAN_POINT ( 'NONE',  ( 39.95015449827720744, -2.613682088886105870, 70.79240656858107172 ) ) ;
#22554 = VECTOR ( 'NONE', #10907, 1000.000000000000227 ) ;
#22555 = VERTEX_POINT ( 'NONE', #5902 ) ;
#22556 = CARTESIAN_POINT ( 'NONE',  ( 43.31606138205698642, -7.467730535347520515, -2.778285769174305919 ) ) ;
#22557 = ORIENTED_EDGE ( 'NONE', *, *, #6948, .F. ) ;
#22558 = CARTESIAN_POINT ( 'NONE',  ( 39.75915168707251723, -2.903840866421913525, 72.49904802271740323 ) ) ;
#22559 = DIRECTION ( 'NONE',  ( 0.000000000000000000, 6.938893903907222067E-15, -1.000000000000000000 ) ) ;
#22560 = CARTESIAN_POINT ( 'NONE',  ( 37.69796330110504101, -7.113682088886100985, 69.66206559358663242 ) ) ;
#22561 = ORIENTED_EDGE ( 'NONE', *, *, #7515, .T. ) ;
#22562 = CARTESIAN_POINT ( 'NONE',  ( 35.86008812008917346, -7.513682088886104893, 71.43714994484035685 ) ) ;
#22563 = VERTEX_POINT ( 'NONE', #22113 ) ;
#22564 = CARTESIAN_POINT ( 'NONE',  ( 39.81606138205699352, 6.191238522346988127, 65.30501292736998664 ) ) ;
#22565 = CARTESIAN_POINT ( 'NONE',  ( 39.37952058850012804, -11.00384086642191050, 71.78268878715392987 ) ) ;
#22566 = CARTESIAN_POINT ( 'NONE',  ( 33.31606138205700773, -11.18542543036242698, 17.47151328161626793 ) ) ;
#22567 = VERTEX_POINT ( 'NONE', #4480 ) ;
#22568 = CARTESIAN_POINT ( 'NONE',  ( 33.81606138205700063, 2.191238522347003226, 70.30501292737000085 ) ) ;
#22569 = DIRECTION ( 'NONE',  ( 0.000000000000000000, 0.5706330172266919076, -0.8212051873014208914 ) ) ;
#22570 = CARTESIAN_POINT ( 'NONE',  ( 39.64521430340305841, -14.80384086642191832, 73.30173637941818754 ) ) ;
#22571 = DIRECTION ( 'NONE',  ( 1.000000000000000000, 1.518641380243644581E-16, 1.055262346480601087E-16 ) ) ;
#22572 = VECTOR ( 'NONE', #18593, 1000.000000000000000 ) ;
#22573 = CARTESIAN_POINT ( 'NONE',  ( 36.87297107704152666, -19.71368208888610951, 72.49904802271740323 ) ) ;
#22574 = FACE_BOUND ( 'NONE', #8225, .T. ) ;
#22575 = FACE_OUTER_BOUND ( 'NONE', #8058, .T. ) ;
#22576 = VECTOR ( 'NONE', #17650, 1000.000000000000000 ) ;
#22577 = ORIENTED_EDGE ( 'NONE', *, *, #2184, .T. ) ;
#22578 = CARTESIAN_POINT ( 'NONE',  ( 35.64099152588523367, 1.392818861812999964, 93.30501292736998664 ) ) ;
#22579 = PLANE ( 'NONE',  #16757 ) ;
#22580 = EDGE_CURVE ( 'NONE', #25158, #2026, #12750, .T. ) ;
#22581 = CARTESIAN_POINT ( 'NONE',  ( 36.68196826583682935, -12.00384086642191228, 70.79240656858107172 ) ) ;
#22582 = DIRECTION ( 'NONE',  ( 1.000000000000000000, 0.000000000000000000, 0.000000000000000000 ) ) ;
#22583 = LINE ( 'NONE', #16786, #17836 ) ;
#22584 = AXIS2_PLACEMENT_3D ( 'NONE', #3322, #16723, #8753 ) ;
#22585 = CARTESIAN_POINT ( 'NONE',  ( 38.93415946300897446, -28.11368208888610098, 73.09843995877328382 ) ) ;
#22586 = CARTESIAN_POINT ( 'NONE',  ( 44.81606138205700063, 28.69846577177642288, 66.12638289304319983 ) ) ;
#22587 = PLANE ( 'NONE',  #3695 ) ;
#22588 = CARTESIAN_POINT ( 'NONE',  ( 38.93415946300896024, -27.50384086642189985, 69.66206559358660400 ) ) ;
#22589 = CARTESIAN_POINT ( 'NONE',  ( 36.72255525790973252, -5.950843403820127442, 82.77262573514066446 ) ) ;
#22590 = AXIS2_PLACEMENT_3D ( 'NONE', #8528, #6587, #14447 ) ;
#22591 =( BOUNDED_CURVE ( )  B_SPLINE_CURVE ( 2, ( #22040, #18060, #20111, #8399, #2447, #17939, #23712, #16109, #6335, #6078, #16240, #21792, #12396, #10324, #8267, #8022, #2071, #4150, #6456, #4528, #14314, #15977, #23834, #6206, #14062, #12019, #5956, #13936, #23961, #20236, #21916, #142, #22163, #19859, #2200, #2574, #9, #7891, #15739, #23589, #256, #9951, #13807, #10081, #12148, #15860, #19987, #21661, #2319, #17811, #11889, #14195, #20367, #12900, #16747, #6703, #20750, #22290, #6963, #18686, #6577, #10834, #22548, #9038, #24460, #20874, #10958, #1023, #2697, #764, #20488, #18811, #10580, #3212, #8655, #18559, #14814, #6832, #14683, #22673, #4651, #4898, #8520, #24715, #8907, #16882, #22802, #14946, #5030, #5164, #18316, #3087, #24582, #13021, #1148, #7090, #637, #8781, #16356, #12649, #18434, #16485, #24204, #14562, #14440, #12529, #24332, #22420, #4771, #2822, #10713, #888, #16617, #12776, #20620, #2952, #13755, #17620, #23524, #7962, #9646, #15925, #19544, #11221, #8084, #15543, #13625, #14008, #10018, #18946, #4090, #1284, #11706, #1748, #11830, #25322, #23781, #5283, #2013, #24847, #9894, #13150, #22921, #21002, #3344, #6020, #17747, #7700, #13877, #15065, #79, #19669, #7222, #19071, #3956, #15677, #2137, #25451, #21861, #11963, #15807, #21610, #23664, #7829, #5762, #206, #1880, #6148, #21732, #19800, #11089, #9764, #23393, #17881, #21477, #9167, #17497, #17013, #5893, #3823, #4214, #10527, #24032, #14381, #4472, #12595, #2266, #8339, #12468, #12083, #10142, #22364, #18132, #8722, #12338, #16181, #18004, #2391, #22235, #16554, #20180, #19931, #22107, #18374, #20430, #6405, #14259, #10652, #14134, #2515, #16428, #6276, #832, #10394, #18256, #20053, #587, #327, #8464, #23905, #16054, #10268, #24404, #457, #21987, #14631, #20313, #8208, #16298, #4723, #24149, #6522, #2645, #2761, #4597, #6645, #705, #8590, #6780, #24279, #14506, #4347, #18501, #12209, #20817, #20688, #19138, #11157, #8851, #1220, #14876, #3283, #25029, #7417, #22737, #3024, #24523, #16690, #1475, #19011, #16818, #3151, #7028, #13089, #15013, #5106, #2890, #10902, #9359, #18754, #17205, #21071, #12713, #12968, #1087, #18622, #22867, #9109, #962, #3415, #11294, #1349, #6901, #9238, #11024, #13222, #7161, #18881, #8972, #17084, #24903, #22487, #20942, #24654, #12838, #7286, #5226, #15135, #22989, #5355, #16948, #24780, #14757, #4840, #10776, #20557, #22614, #4970, #44 ),
 .UNSPECIFIED., .F., .T. ) 
 B_SPLINE_CURVE_WITH_KNOTS ( ( 3, 2, 2, 2, 2, 2, 2, 2, 2, 2, 2, 2, 2, 2, 2, 2, 2, 2, 2, 2, 2, 2, 2, 2, 2, 2, 2, 2, 2, 2, 2, 2, 2, 2, 2, 2, 2, 2, 2, 2, 2, 2, 2, 2, 2, 2, 2, 2, 2, 2, 2, 2, 2, 2, 2, 2, 2, 2, 2, 2, 2, 2, 2, 2, 2, 2, 2, 2, 2, 2, 2, 2, 2, 2, 2, 2, 2, 2, 2, 2, 2, 2, 2, 2, 2, 2, 2, 2, 2, 2, 2, 2, 2, 2, 2, 2, 2, 2, 2, 2, 2, 2, 2, 2, 2, 2, 2, 2, 2, 2, 2, 2, 2, 2, 2, 2, 2, 2, 2, 2, 2, 2, 2, 2, 2, 2, 2, 2, 2, 2, 2, 2, 2, 2, 2, 2, 2, 2, 2, 2, 2, 2, 2, 2, 2, 2, 2, 2, 2, 2, 2, 2, 2, 2, 3 ),
 ( 0.008536090408176065514, 0.01250000000000000069, 0.01874999999999999931, 0.02500000000000000139, 0.03125000000000000000, 0.03749999999999999861, 0.04374999999999999722, 0.05000000000000000278, 0.05625000000000000139, 0.06250000000000000000, 0.06875000000000000555, 0.07500000000000001110, 0.08125000000000001665, 0.08749999999999999445, 0.09375000000000000000, 0.1000000000000000056, 0.1062500000000000111, 0.1125000000000000167, 0.1187499999999999944, 0.1250000000000000000, 0.1312500000000000056, 0.1375000000000000111, 0.1437499999999999889, 0.1499999999999999944, 0.1562500000000000000, 0.1625000000000000056, 0.1687500000000000111, 0.1749999999999999889, 0.1812499999999999944, 0.1875000000000000000, 0.1937500000000000056, 0.2000000000000000111, 0.2062499999999999889, 0.2124999999999999944, 0.2187500000000000000, 0.2250000000000000056, 0.2312500000000000111, 0.2374999999999999889, 0.2437499999999999944, 0.2500000000000000000, 0.2562499999999999778, 0.2625000000000000111, 0.2687499999999999889, 0.2750000000000000222, 0.2812500000000000000, 0.2874999999999999778, 0.2937500000000000111, 0.2999999999999999889, 0.3062500000000000222, 0.3124999999999999445, 0.3187499999999999778, 0.3250000000000000111, 0.3312499999999999889, 0.3375000000000000222, 0.3437500000000000000, 0.3499999999999999778, 0.3562500000000000111, 0.3624999999999999889, 0.3687500000000000222, 0.3750000000000000000, 0.3812499999999999778, 0.3875000000000000111, 0.3937499999999999889, 0.4000000000000000222, 0.4062500000000000000, 0.4124999999999999778, 0.4187500000000000111, 0.4249999999999999889, 0.4312500000000000222, 0.4375000000000000000, 0.4437500000000000333, 0.4500000000000000111, 0.4562499999999999889, 0.4625000000000000222, 0.4687500000000000000, 0.4749999999999999778, 0.4812500000000000111, 0.4874999999999999889, 0.4937500000000000222, 0.5000000000000000000, 0.5062499999999999778, 0.5124999999999999556, 0.5187500000000000444, 0.5250000000000000222, 0.5312500000000000000, 0.5374999999999999778, 0.5437499999999999556, 0.5500000000000000444, 0.5562500000000000222, 0.5625000000000000000, 0.5687499999999999778, 0.5749999999999999556, 0.5812500000000000444, 0.5875000000000000222, 0.5937500000000000000, 0.5999999999999999778, 0.6062499999999999556, 0.6125000000000000444, 0.6187500000000000222, 0.6250000000000000000, 0.6312499999999999778, 0.6374999999999999556, 0.6437500000000000444, 0.6500000000000000222, 0.6562500000000000000, 0.6624999999999999778, 0.6687499999999999556, 0.6750000000000000444, 0.6812500000000000222, 0.6875000000000000000, 0.6937500000000000888, 0.6999999999999999556, 0.7062500000000000444, 0.7125000000000000222, 0.7187500000000000000, 0.7249999999999999778, 0.7312499999999999556, 0.7375000000000000444, 0.7437500000000000222, 0.7500000000000000000, 0.7562499999999999778, 0.7624999999999999556, 0.7687500000000000444, 0.7750000000000000222, 0.7812500000000000000, 0.7874999999999999778, 0.7937499999999999556, 0.7999999999999999334, 0.8062500000000000222, 0.8125000000000000000, 0.8187499999999999778, 0.8249999999999999556, 0.8312500000000000444, 0.8375000000000000222, 0.8437500000000000000, 0.8499999999999999778, 0.8562499999999999556, 0.8625000000000000444, 0.8687500000000000222, 0.8750000000000000000, 0.8812499999999999778, 0.8874999999999999556, 0.8937500000000000444, 0.9000000000000000222, 0.9062500000000000000, 0.9124999999999999778, 0.9187499999999999556, 0.9250000000000000444, 0.9312500000000000222, 0.9375000000000000000, 0.9437499999999999778, 0.9499999999999999556, 0.9562500000000000444, 0.9625000000000000222, 0.9687500000000000000 ),
 .UNSPECIFIED. ) 
 CURVE ( )  GEOMETRIC_REPRESENTATION_ITEM ( )  RATIONAL_B_SPLINE_CURVE ( ( 0.9772918381245772057, 0.9689587928776128845, 1.000000000000000000, 0.9510565162951535312, 1.000000000000000000, 0.9510565162951535312, 1.000000000000000000, 0.9510565162951535312, 1.000000000000000000, 0.9510565162951535312, 1.000000000000000000, 0.9510565162951535312, 1.000000000000000000, 0.9510565162951535312, 1.000000000000000000, 0.9510565162951535312, 1.000000000000000000, 0.9510565162951535312, 1.000000000000000000, 0.9510565162951535312, 1.000000000000000000, 0.9510565162951535312, 1.000000000000000000, 0.9510565162951535312, 1.000000000000000000, 0.9510565162951535312, 1.000000000000000000, 0.9510565162951535312, 1.000000000000000000, 0.9510565162951535312, 1.000000000000000000, 0.9510565162951535312, 1.000000000000000000, 0.9510565162951535312, 1.000000000000000000, 0.9510565162951535312, 1.000000000000000000, 0.9510565162951535312, 1.000000000000000000, 0.9510565162951535312, 1.000000000000000000, 0.9510565162951535312, 1.000000000000000000, 0.9510565162951535312, 1.000000000000000000, 0.9510565162951535312, 1.000000000000000000, 0.9510565162951535312, 1.000000000000000000, 0.9510565162951535312, 1.000000000000000000, 0.9510565162951535312, 1.000000000000000000, 0.9510565162951535312, 1.000000000000000000, 0.9510565162951535312, 1.000000000000000000, 0.9510565162951535312, 1.000000000000000000, 0.9510565162951535312, 1.000000000000000000, 0.9510565162951535312, 1.000000000000000000, 0.9510565162951535312, 1.000000000000000000, 0.9510565162951535312, 1.000000000000000000, 0.9510565162951535312, 1.000000000000000000, 0.9510565162951535312, 1.000000000000000000, 0.9510565162951535312, 1.000000000000000000, 0.9510565162951535312, 1.000000000000000000, 0.9510565162951535312, 1.000000000000000000, 0.9510565162951535312, 1.000000000000000000, 0.9510565162951535312, 1.000000000000000000, 0.9510565162951535312, 1.000000000000000000, 0.9510565162951535312, 1.000000000000000000, 0.9510565162951535312, 1.000000000000000000, 0.9510565162951535312, 1.000000000000000000, 0.9510565162951535312, 1.000000000000000000, 0.9510565162951535312, 1.000000000000000000, 0.9510565162951535312, 1.000000000000000000, 0.9510565162951535312, 1.000000000000000000, 0.9510565162951535312, 1.000000000000000000, 0.9510565162951535312, 1.000000000000000000, 0.9510565162951535312, 1.000000000000000000, 0.9510565162951535312, 1.000000000000000000, 0.9510565162951535312, 1.000000000000000000, 0.9510565162951535312, 1.000000000000000000, 0.9510565162951535312, 1.000000000000000000, 0.9510565162951535312, 1.000000000000000000, 0.9510565162951535312, 1.000000000000000000, 0.9510565162951535312, 1.000000000000000000, 0.9510565162951535312, 1.000000000000000000, 0.9510565162951535312, 1.000000000000000000, 0.9510565162951535312, 1.000000000000000000, 0.9510565162951535312, 1.000000000000000000, 0.9510565162951535312, 1.000000000000000000, 0.9510565162951535312, 1.000000000000000000, 0.9510565162951535312, 1.000000000000000000, 0.9510565162951535312, 1.000000000000000000, 0.9510565162951535312, 1.000000000000000000, 0.9510565162951535312, 1.000000000000000000, 0.9510565162951535312, 1.000000000000000000, 0.9510565162951535312, 1.000000000000000000, 0.9510565162951535312, 1.000000000000000000, 0.9510565162951535312, 1.000000000000000000, 0.9510565162951535312, 1.000000000000000000, 0.9510565162951535312, 1.000000000000000000, 0.9510565162951535312, 1.000000000000000000, 0.9510565162951535312, 1.000000000000000000, 0.9510565162951535312, 1.000000000000000000, 0.9510565162951535312, 1.000000000000000000, 0.9510565162951535312, 1.000000000000000000, 0.9510565162951535312, 1.000000000000000000, 0.9510565162951535312, 1.000000000000000000, 0.9510565162951535312, 1.000000000000000000, 0.9510565162951535312, 1.000000000000000000, 0.9510565162951535312, 1.000000000000000000, 0.9510565162951535312, 1.000000000000000000, 0.9510565162951535312, 1.000000000000000000, 0.9510565162951535312, 1.000000000000000000, 0.9510565162951535312, 1.000000000000000000, 0.9510565162951535312, 1.000000000000000000, 0.9510565162951535312, 1.000000000000000000, 0.9510565162951535312, 1.000000000000000000, 0.9510565162951535312, 1.000000000000000000, 0.9510565162951535312, 1.000000000000000000, 0.9510565162951535312, 1.000000000000000000, 0.9510565162951535312, 1.000000000000000000, 0.9510565162951535312, 1.000000000000000000, 0.9510565162951535312, 1.000000000000000000, 0.9510565162951535312, 1.000000000000000000, 0.9510565162951535312, 1.000000000000000000, 0.9510565162951535312, 1.000000000000000000, 0.9510565162951535312, 1.000000000000000000, 0.9510565162951535312, 1.000000000000000000, 0.9510565162951535312, 1.000000000000000000, 0.9510565162951535312, 1.000000000000000000, 0.9510565162951535312, 1.000000000000000000, 0.9510565162951535312, 1.000000000000000000, 0.9510565162951535312, 1.000000000000000000, 0.9510565162951535312, 1.000000000000000000, 0.9510565162951535312, 1.000000000000000000, 0.9510565162951535312, 1.000000000000000000, 0.9510565162951535312, 1.000000000000000000, 0.9510565162951535312, 1.000000000000000000, 0.9510565162951535312, 1.000000000000000000, 0.9510565162951535312, 1.000000000000000000, 0.9510565162951535312, 1.000000000000000000, 0.9510565162951535312, 1.000000000000000000, 0.9510565162951535312, 1.000000000000000000, 0.9510565162951535312, 1.000000000000000000, 0.9510565162951535312, 1.000000000000000000, 0.9510565162951535312, 1.000000000000000000, 0.9510565162951535312, 1.000000000000000000, 0.9510565162951535312, 1.000000000000000000, 0.9510565162951535312, 1.000000000000000000, 0.9510565162951535312, 1.000000000000000000, 0.9510565162951535312, 1.000000000000000000, 0.9510565162951535312, 1.000000000000000000, 0.9510565162951535312, 1.000000000000000000, 0.9510565162951535312, 1.000000000000000000, 0.9510565162951535312, 1.000000000000000000, 0.9510565162951535312, 1.000000000000000000, 0.9510565162951535312, 1.000000000000000000, 0.9510565162951535312, 1.000000000000000000, 0.9510565162951535312, 1.000000000000000000, 0.9510565162951535312, 1.000000000000000000, 0.9510565162951535312, 1.000000000000000000, 0.9510565162951535312, 1.000000000000000000, 0.9510565162951535312, 1.000000000000000000, 0.9510565162951535312, 1.000000000000000000, 0.9510565162951535312, 1.000000000000000000, 0.9510565162951535312, 1.000000000000000000, 0.9510565162951535312, 1.000000000000000000, 0.9510565162951535312, 1.000000000000000000, 0.9510565162951535312, 1.000000000000000000, 0.9510565162951535312, 1.000000000000000000, 0.9510565162951535312, 1.000000000000000000, 0.9510565162951535312, 1.000000000000000000, 0.9510565162951535312, 1.000000000000000000, 0.9510565162951535312, 1.000000000000000000, 0.9510565162951535312, 1.000000000000000000, 0.9510565162951535312, 1.000000000000000000, 0.9510565162951535312, 1.000000000000000000, 0.9510565162951535312, 1.000000000000000000, 0.9510565162951535312, 1.000000000000000000, 0.9510565162951535312, 1.000000000000000000 ) ) 
 REPRESENTATION_ITEM ( '' )  );
#22592 = CARTESIAN_POINT ( 'NONE',  ( 37.80618814713140097, -21.91368208888610880, 73.13360434286903455 ) ) ;
#22593 = ORIENTED_EDGE ( 'NONE', *, *, #12827, .F. ) ;
#22594 = ORIENTED_EDGE ( 'NONE', *, *, #2009, .F. ) ;
#22595 = CARTESIAN_POINT ( 'NONE',  ( 45.81606138205700063, 40.39281886181299797, 84.30501292736984453 ) ) ;
#22596 = PLANE ( 'NONE',  #21983 ) ;
#22597 = CARTESIAN_POINT ( 'NONE',  ( 39.02742774030102879, -2.213682088886101518, 72.26730301774236409 ) ) ;
#22598 = VECTOR ( 'NONE', #5657, 1000.000000000000000 ) ;
#22599 = CARTESIAN_POINT ( 'NONE',  ( 38.63098279924290068, -28.70384086642190979, 72.53360434286901182 ) ) ;
#22600 = ORIENTED_EDGE ( 'NONE', *, *, #17453, .F. ) ;
#22601 = EDGE_LOOP ( 'NONE', ( #19149, #18357, #5381, #2223 ) ) ;
#22602 = DIRECTION ( 'NONE',  ( -2.122643018205887308E-17, 1.000000000000000000, -3.120611096041553009E-15 ) ) ;
#22603 = CARTESIAN_POINT ( 'NONE',  ( 46.81606138205706458, -34.55876147768182705, 70.30501292735635843 ) ) ;
#22604 = ORIENTED_EDGE ( 'NONE', *, *, #25171, .F. ) ;
#22605 = CARTESIAN_POINT ( 'NONE',  ( 36.68196826583682935, -4.003840866421911393, 70.79240656858108593 ) ) ;
#22606 = CIRCLE ( 'NONE', #18916, 3.000000000000002665 ) ;
#22607 = AXIS2_PLACEMENT_3D ( 'NONE', #16583, #22643, #8998 ) ;
#22608 = CARTESIAN_POINT ( 'NONE',  ( 43.31606138205700063, -35.70002751211045933, 71.94742330197156832 ) ) ;
#22609 = CARTESIAN_POINT ( 'NONE',  ( 40.64099152588523367, -8.607181138186998481, 88.30501292736998664 ) ) ;
#22610 = VERTEX_POINT ( 'NONE', #16302 ) ;
#22611 = ORIENTED_EDGE ( 'NONE', *, *, #22948, .F. ) ;
#22612 = VECTOR ( 'NONE', #23151, 1000.000000000000000 ) ;
#22613 = DIRECTION ( 'NONE',  ( 0.000000000000000000, 0.8212051873014208914, 0.5706330172266919076 ) ) ;
#22614 = CARTESIAN_POINT ( 'NONE',  ( 39.38009889167650357, 1.786317911113891821, 72.75271321436734695 ) ) ;
#22615 = CARTESIAN_POINT ( 'NONE',  ( 40.64099152588522657, 1.142818861812999742, 84.30501292737000085 ) ) ;
#22616 =( LENGTH_UNIT ( ) NAMED_UNIT ( * ) SI_UNIT ( .MILLI., .METRE. ) );
#22617 = DIRECTION ( 'NONE',  ( 0.000000000000000000, -0.5706330172266920187, 0.8212051873014210024 ) ) ;
#22618 = VECTOR ( 'NONE', #5710, 1000.000000000000000 ) ;
#22619 = LINE ( 'NONE', #4975, #2793 ) ;
#22620 = CARTESIAN_POINT ( 'NONE',  ( 43.23254934194437027, 3.260207155506757992, 6.242825920358057168 ) ) ;
#22621 = AXIS2_PLACEMENT_3D ( 'NONE', #3731, #2051, #11607 ) ;
#22622 = CARTESIAN_POINT ( 'NONE',  ( 31.81606138205700418, 35.44123852234597649, 68.80501292736990138 ) ) ;
#22623 = DIRECTION ( 'NONE',  ( -1.849283715844614456E-16, 0.8212051873014208914, 0.5706330172266919076 ) ) ;
#22624 = DIRECTION ( 'NONE',  ( 0.000000000000000000, 1.000000000000000000, 0.000000000000000000 ) ) ;
#22625 = ORIENTED_EDGE ( 'NONE', *, *, #250, .F. ) ;
#22626 = VERTEX_POINT ( 'NONE', #9901 ) ;
#22627 = CARTESIAN_POINT ( 'NONE',  ( 40.31606138205700773, -31.05876147765399864, 75.30501292737010033 ) ) ;
#22628 = LINE ( 'NONE', #5372, #18504 ) ;
#22629 = EDGE_CURVE ( 'NONE', #5497, #180, #2022, .T. ) ;
#22630 = ADVANCED_FACE ( 'NONE', ( #4097 ), #24153, .F. ) ;
#22631 = CARTESIAN_POINT ( 'NONE',  ( 38.73920764526925353, -16.11368208888610454, 72.49843995877330372 ) ) ;
#22632 = ORIENTED_EDGE ( 'NONE', *, *, #5298, .T. ) ;
#22633 = EDGE_LOOP ( 'NONE', ( #25210, #4027, #14628, #13598 ) ) ;
#22634 = LINE ( 'NONE', #7435, #11643 ) ;
#22635 = CARTESIAN_POINT ( 'NONE',  ( 39.98359781491296161, -4.413682088886105248, 71.86517103874048473 ) ) ;
#22636 = CARTESIAN_POINT ( 'NONE',  ( 39.29254315202757653, -22.80384086642191477, 72.81632618279321889 ) ) ;
#22637 = EDGE_CURVE ( 'NONE', #16151, #18901, #10275, .T. ) ;
#22638 = EDGE_CURVE ( 'NONE', #19362, #2254, #4602, .T. ) ;
#22639 = AXIS2_PLACEMENT_3D ( 'NONE', #12006, #2434, #16341 ) ;
#22640 = CARTESIAN_POINT ( 'NONE',  ( 40.64099152588522657, 1.142818861812999742, 82.55501292736997243 ) ) ;
#22641 = CARTESIAN_POINT ( 'NONE',  ( 39.02088643472237095, -8.913682088886103472, 69.02690120949094421 ) ) ;
#22642 = AXIS2_PLACEMENT_3D ( 'NONE', #16306, #21997, #8599 ) ;
#22643 = DIRECTION ( 'NONE',  ( 1.327674326049719602E-15, -0.4425581086832399147, 0.8967398287344627850 ) ) ;
#22644 = CARTESIAN_POINT ( 'NONE',  ( 40.11623881305710881, -6.323019409765026744, 83.24594533976426192 ) ) ;
#22645 = EDGE_CURVE ( 'NONE', #10246, #19039, #17257, .T. ) ;
#22646 = FACE_BOUND ( 'NONE', #6653, .T. ) ;
#22647 = EDGE_CURVE ( 'NONE', #23614, #20521, #4222, .T. ) ;
#22648 = DIRECTION ( 'NONE',  ( 1.000000000000000000, -3.083952846180990083E-15, 9.251858538542970050E-30 ) ) ;
#22649 = CARTESIAN_POINT ( 'NONE',  ( 40.31606138205700773, -7.108955154158179468, 82.62193108360246185 ) ) ;
#22650 = CARTESIAN_POINT ( 'NONE',  ( 40.06606138205700063, 5.594015759443068170, 2.006005027196319901 ) ) ;
#22651 = FACE_OUTER_BOUND ( 'NONE', #17535, .T. ) ;
#22652 = ORIENTED_EDGE ( 'NONE', *, *, #6983, .T. ) ;
#22653 = VECTOR ( 'NONE', #1273, 1000.000000000000000 ) ;
#22654 = DIRECTION ( 'NONE',  ( 8.758115402030106693E-47, -1.000000000000000000, 3.469446951953613400E-15 ) ) ;
#22655 = DIRECTION ( 'NONE',  ( -1.000000000000000000, 5.204170427930413997E-31, 1.734723475976804876E-16 ) ) ;
#22656 = ORIENTED_EDGE ( 'NONE', *, *, #13903, .T. ) ;
#22657 = EDGE_LOOP ( 'NONE', ( #20257, #3974, #22213, #14907 ) ) ;
#22658 = UNCERTAINTY_MEASURE_WITH_UNIT (LENGTH_MEASURE( 1.000000000000000082E-05 ), #18674, 'distance_accuracy_value', 'NONE');
#22659 = AXIS2_PLACEMENT_3D ( 'NONE', #2899, #16564, #24416 ) ;
#22660 = CARTESIAN_POINT ( 'NONE',  ( 40.55423172469004101, -15.20384086642191512, 70.70992431699450265 ) ) ;
#22661 = CARTESIAN_POINT ( 'NONE',  ( 39.29254315202756231, -18.81368208888610027, 69.94417936956672577 ) ) ;
#22662 = CARTESIAN_POINT ( 'NONE',  ( 43.31606138205700773, -19.92642959707777806, 24.72592537066031682 ) ) ;
#22663 = LINE ( 'NONE', #6951, #21307 ) ;
#22664 = ORIENTED_EDGE ( 'NONE', *, *, #10244, .F. ) ;
#22665 = DIRECTION ( 'NONE',  ( 0.000000000000000000, -0.8212051873014223347, -0.5706330172266899092 ) ) ;
#22666 = DIRECTION ( 'NONE',  ( -1.000000000000000000, -1.052872940142565459E-15, -1.848188032574765003E-17 ) ) ;
#22667 = CARTESIAN_POINT ( 'NONE',  ( 40.33642880535524000, -26.31368208888610383, 72.77780686321125359 ) ) ;
#22668 = ORIENTED_EDGE ( 'NONE', *, *, #19311, .F. ) ;
#22669 = DIRECTION ( 'NONE',  ( -1.000000000000000000, -3.091505625455828697E-15, -4.515976121274772923E-17 ) ) ;
#22670 = FACE_OUTER_BOUND ( 'NONE', #1012, .T. ) ;
#22671 = CARTESIAN_POINT ( 'NONE',  ( 36.68196826583682935, -1.613682088886104982, 71.96809898377890136 ) ) ;
#22672 = CARTESIAN_POINT ( 'NONE',  ( 42.56606138205700063, -33.77966242919868733, 58.66916295099436951 ) ) ;
#22673 = CARTESIAN_POINT ( 'NONE',  ( 38.82593461698262871, -20.91368208888609814, 69.62690120949091011 ) ) ;
#22674 = AXIS2_PLACEMENT_3D ( 'NONE', #4203, #2126, #6012 ) ;
#22675 = CARTESIAN_POINT ( 'NONE',  ( 40.31606138205700773, -20.32127907754186680, 75.99695190479390305 ) ) ;
#22676 = CARTESIAN_POINT ( 'NONE',  ( 44.81606138205700063, -25.52563857111379875, 92.39878177866870601 ) ) ;
#22677 = CARTESIAN_POINT ( 'NONE',  ( 37.12184278917507640, -18.10384086642191193, 71.32335560751961623 ) ) ;
#22678 = CARTESIAN_POINT ( 'NONE',  ( 39.29254315202756231, -8.813682088886100274, 69.94417936956673998 ) ) ;
#22679 = EDGE_LOOP ( 'NONE', ( #19586, #22593, #77, #21882 ) ) ;
#22680 = DIRECTION ( 'NONE',  ( 1.000000000000000000, 1.115287202090205222E-30, -1.734723475976805122E-15 ) ) ;
#22681 = ADVANCED_FACE ( 'NONE', ( #12215 ), #17753, .F. ) ;
#22682 = ORIENTED_EDGE ( 'NONE', *, *, #900, .F. ) ;
#22683 = CARTESIAN_POINT ( 'NONE',  ( 39.82603832034400426, -7.303840866421906775, 70.35351908239857721 ) ) ;
#22684 = CARTESIAN_POINT ( 'NONE',  ( 36.31606138205700063, 42.19123852234596939, 65.30501292736988717 ) ) ;
#22685 = CARTESIAN_POINT ( 'NONE',  ( 39.95015449827720744, -2.613682088886105870, 70.79240656858107172 ) ) ;
#22686 = EDGE_LOOP ( 'NONE', ( #12664, #2365, #13732, #22957, #18512, #18605, #22851, #12771, #12637, #10215, #22210 ) ) ;
#22687 = CARTESIAN_POINT ( 'NONE',  ( 40.26954217208371034, -8.713682088886100630, 69.89063713639259845 ) ) ;
#22688 = ORIENTED_EDGE ( 'NONE', *, *, #25106, .T. ) ;
#22689 = DIRECTION ( 'NONE',  ( -1.734723475976805122E-16, 0.000000000000000000, -1.000000000000000000 ) ) ;
#22690 = CARTESIAN_POINT ( 'NONE',  ( 37.38336156205273397, -9.903840866421909084, 70.63227792289248441 ) ) ;
#22691 = CARTESIAN_POINT ( 'NONE',  ( 33.40064408022072939, 40.76768529863396395, 79.57823623207323749 ) ) ;
#22692 = ORIENTED_EDGE ( 'NONE', *, *, #25372, .F. ) ;
#22693 = DIRECTION ( 'NONE',  ( -1.000000000000000000, 1.115179377413661005E-30, 3.717264591378870232E-16 ) ) ;
#22694 = LINE ( 'NONE', #7244, #19870 ) ;
#22695 = AXIS2_PLACEMENT_3D ( 'NONE', #18836, #1176, #20902 ) ;
#22696 = CARTESIAN_POINT ( 'NONE',  ( 39.12911128074872380, -13.50384086642191228, 69.06206559358665231 ) ) ;
#22697 = CARTESIAN_POINT ( 'NONE',  ( 37.09113907096683960, -21.80780096054036221, 75.31329243205692592 ) ) ;
#22698 = CYLINDRICAL_SURFACE ( 'NONE', #22695, 0.4999999999999998890 ) ;
#22699 = CARTESIAN_POINT ( 'NONE',  ( 36.49096545463212493, -23.51368208888609601, 71.43714994484030001 ) ) ;
#22700 = DIRECTION ( 'NONE',  ( -1.734723475976814737E-16, 1.000000000000000000, -3.491481338843135327E-15 ) ) ;
#22701 = FACE_OUTER_BOUND ( 'NONE', #23062, .T. ) ;
#22702 = ORIENTED_EDGE ( 'NONE', *, *, #9675, .F. ) ;
#22703 = CYLINDRICAL_SURFACE ( 'NONE', #132, 1.750000000000001554 ) ;
#22704 = CARTESIAN_POINT ( 'NONE',  ( 45.81606138205707879, -39.99575152356564445, 63.13209164280871022 ) ) ;
#22705 = VECTOR ( 'NONE', #14127, 1000.000000000000114 ) ;
#22706 = CARTESIAN_POINT ( 'NONE',  ( 39.95015449827720744, -7.003840866421910505, 71.96809898377888715 ) ) ;
#22707 = VECTOR ( 'NONE', #11461, 1000.000000000000000 ) ;
#22708 = EDGE_CURVE ( 'NONE', #23863, #20356, #2398, .T. ) ;
#22709 = LINE ( 'NONE', #2859, #11678 ) ;
#22710 = CARTESIAN_POINT ( 'NONE',  ( 39.29254315202756231, -22.81368208888610027, 69.94417936956672577 ) ) ;
#22711 = EDGE_CURVE ( 'NONE', #16812, #23473, #2143, .T. ) ;
#22712 = CARTESIAN_POINT ( 'NONE',  ( 40.31606138205700773, -16.48551471403133206, 77.11349248448009064 ) ) ;
#22713 = EDGE_CURVE ( 'NONE', #14645, #3435, #10026, .T. ) ;
#22714 = TOROIDAL_SURFACE ( 'NONE', #20661, 1.000000000000000000, 1.000000000000000000 ) ;
#22715 = CARTESIAN_POINT ( 'NONE',  ( 39.75915168707251723, -26.90384086642191619, 72.49904802271737481 ) ) ;
#22716 = LINE ( 'NONE', #809, #19629 ) ;
#22717 = CARTESIAN_POINT ( 'NONE',  ( 39.38009889167650357, -26.21368208888610951, 72.75271321436730432 ) ) ;
#22718 = ORIENTED_EDGE ( 'NONE', *, *, #17453, .T. ) ;
#22719 = VERTEX_POINT ( 'NONE', #17887 ) ;
#22720 = CARTESIAN_POINT ( 'NONE',  ( 45.81606138205700063, 40.39281886181299797, 66.30501292737000085 ) ) ;
#22721 = DIRECTION ( 'NONE',  ( -1.000000000000000000, -1.000000000000000078E-15, 0.000000000000000000 ) ) ;
#22722 = CARTESIAN_POINT ( 'NONE',  ( 37.89291511884479036, -28.50384086642191406, 72.49843995877328950 ) ) ;
#22723 = CARTESIAN_POINT ( 'NONE',  ( 39.31564783533280405, 1.686317911113899282, 72.03616607671141026 ) ) ;
#22724 = ORIENTED_EDGE ( 'NONE', *, *, #12078, .T. ) ;
#22725 = EDGE_LOOP ( 'NONE', ( #19967, #1298, #16573, #2680 ) ) ;
#22726 = CARTESIAN_POINT ( 'NONE',  ( 31.81606138205700418, 40.39281886181299797, 81.75501292736983316 ) ) ;
#22727 = CARTESIAN_POINT ( 'NONE',  ( 43.81606138205700063, 4.103895195095678794, 6.341006091748962348 ) ) ;
#22728 = VERTEX_POINT ( 'NONE', #2522 ) ;
#22729 = CARTESIAN_POINT ( 'NONE',  ( 36.87297107704149823, -3.903840866421907752, 70.26145752964255564 ) ) ;
#22730 = AXIS2_PLACEMENT_3D ( 'NONE', #15679, #21479, #1752 ) ;
#22731 = CARTESIAN_POINT ( 'NONE',  ( 36.06606138205700063, 2.740850673309605412, 6.112030963703427133 ) ) ;
#22732 = AXIS2_PLACEMENT_3D ( 'NONE', #5505, #1107, #18902 ) ;
#22733 = CARTESIAN_POINT ( 'NONE',  ( 43.31606138205700063, 3.296535697557910538, 65.33616386252352015 ) ) ;
#22734 = ORIENTED_EDGE ( 'NONE', *, *, #12044, .F. ) ;
#22735 = VERTEX_POINT ( 'NONE', #6411 ) ;
#22736 = CARTESIAN_POINT ( 'NONE',  ( 30.81606138205697576, -4.349482454670884124, -5.142398479549302515 ) ) ;
#22737 = CARTESIAN_POINT ( 'NONE',  ( 36.64852494920107517, -3.413682088886104360, 70.89533451361948835 ) ) ;
#22738 = AXIS2_PLACEMENT_3D ( 'NONE', #17522, #21373, #1781 ) ;
#22739 = CIRCLE ( 'NONE', #14923, 9.500000000000001776 ) ;
#22740 = DIRECTION ( 'NONE',  ( 0.000000000000000000, -0.6568589528324746407, 0.7540134720837717852 ) ) ;
#22741 = DIRECTION ( 'NONE',  ( -1.000000000000000000, 0.000000000000000000, 0.000000000000000000 ) ) ;
#22742 = EDGE_LOOP ( 'NONE', ( #8096, #11358, #13729, #24595, #7872, #1237, #23281, #22864, #9222, #2803, #2838, #7654 ) ) ;
#22743 = CARTESIAN_POINT ( 'NONE',  ( 42.99361969242278292, 2.839052459004266726, 6.102834979010582472 ) ) ;
#22744 = AXIS2_PLACEMENT_3D ( 'NONE', #21560, #5588, #11277 ) ;
#22745 = LINE ( 'NONE', #6908, #10037 ) ;
#22746 = VECTOR ( 'NONE', #23115, 1000.000000000000000 ) ;
#22747 = CARTESIAN_POINT ( 'NONE',  ( 33.56606138205700773, -38.55876147765401640, 71.30501292737012875 ) ) ;
#22748 = PLANE ( 'NONE',  #8165 ) ;
#22749 = VECTOR ( 'NONE', #10891, 1000.000000000000000 ) ;
#22750 = LINE ( 'NONE', #14638, #23476 ) ;
#22751 = ORIENTED_EDGE ( 'NONE', *, *, #2275, .T. ) ;
#22752 = VERTEX_POINT ( 'NONE', #10402 ) ;
#22753 = DIRECTION ( 'NONE',  ( 1.734723475976804876E-16, 3.491481338843135327E-15, 1.000000000000000000 ) ) ;
#22754 = CARTESIAN_POINT ( 'NONE',  ( 32.81606138205700773, 44.92314894770294131, 80.37823623207322044 ) ) ;
#22755 = CARTESIAN_POINT ( 'NONE',  ( 39.24876120206128860, -14.71368208888610241, 70.63227792289245599 ) ) ;
#22756 = VERTEX_POINT ( 'NONE', #214 ) ;
#22757 = VECTOR ( 'NONE', #13624, 1000.000000000000000 ) ;
#22758 = EDGE_LOOP ( 'NONE', ( #23884, #16980, #8758, #1404 ) ) ;
#22759 = EDGE_CURVE ( 'NONE', #11945, #18026, #14388, .T. ) ;
#22760 = FACE_OUTER_BOUND ( 'NONE', #2114, .T. ) ;
#22761 = CARTESIAN_POINT ( 'NONE',  ( 37.80618814713140097, -1.913682088886106136, 73.13360434286904876 ) ) ;
#22762 = CARTESIAN_POINT ( 'NONE',  ( 36.64852494920107517, -22.20384086642191335, 71.86517103874048473 ) ) ;
#22763 = CARTESIAN_POINT ( 'NONE',  ( 44.81606138205700063, 34.87886987267150118, 81.44836866983821722 ) ) ;
#22764 = CARTESIAN_POINT ( 'NONE',  ( 36.11133435605973574, -7.613682088886103649, 72.15350918040385864 ) ) ;
#22765 = AXIS2_PLACEMENT_3D ( 'NONE', #17816, #15744, #10085 ) ;
#22766 = CARTESIAN_POINT ( 'NONE',  ( 45.81606138205706458, -34.13844651005145181, 70.48338531520533934 ) ) ;
#22767 = VERTEX_POINT ( 'NONE', #85 ) ;
#22768 = DIRECTION ( 'NONE',  ( 1.000000000000000000, -0.000000000000000000, 0.000000000000000000 ) ) ;
#22769 = CIRCLE ( 'NONE', #543, 0.4999999999999982792 ) ;
#22770 = CARTESIAN_POINT ( 'NONE',  ( 40.56606138205700773, 2.740850673309605412, 6.112030963703427133 ) ) ;
#22771 = DIRECTION ( 'NONE',  ( 1.000000000000000000, 2.611101091812726599E-15, -1.919289851541777660E-16 ) ) ;
#22772 = ADVANCED_FACE ( 'NONE', ( #18266 ), #15931, .F. ) ;
#22773 = EDGE_CURVE ( 'NONE', #10464, #9429, #8215, .T. ) ;
#22774 = CARTESIAN_POINT ( 'NONE',  ( 40.25357836725066818, -6.620766072854777917, 82.70492630226405595 ) ) ;
#22775 = VECTOR ( 'NONE', #15573, 1000.000000000000000 ) ;
#22776 = DIRECTION ( 'NONE',  ( 1.000000000000000000, 0.000000000000000000, 0.000000000000000000 ) ) ;
#22777 = ADVANCED_FACE ( 'NONE', ( #23912 ), #7970, .T. ) ;
#22778 = FACE_OUTER_BOUND ( 'NONE', #13167, .T. ) ;
#22779 = EDGE_CURVE ( 'NONE', #22879, #22231, #24039, .T. ) ;
#22780 = ORIENTED_EDGE ( 'NONE', *, *, #796, .F. ) ;
#22781 = DIRECTION ( 'NONE',  ( 1.000000000000000000, -0.000000000000000000, 0.000000000000000000 ) ) ;
#22782 = DIRECTION ( 'NONE',  ( 1.000000000000000000, 2.999999999999999839E-15, 0.000000000000000000 ) ) ;
#22783 = ORIENTED_EDGE ( 'NONE', *, *, #25221, .F. ) ;
#22784 = EDGE_LOOP ( 'NONE', ( #16729, #15906, #8922, #23799 ) ) ;
#22785 = VECTOR ( 'NONE', #893, 1000.000000000000000 ) ;
#22786 = CARTESIAN_POINT ( 'NONE',  ( 36.98690846071097127, -19.80384086642191477, 69.45876917294175712 ) ) ;
#22787 = CIRCLE ( 'NONE', #18281, 0.9999999999999940048 ) ;
#22788 = AXIS2_PLACEMENT_3D ( 'NONE', #15005, #25023, #19002 ) ;
#22789 = EDGE_CURVE ( 'NONE', #6972, #5864, #18379, .T. ) ;
#22790 = CARTESIAN_POINT ( 'NONE',  ( 37.69796330110504101, -23.11368208888609743, 69.66206559358660400 ) ) ;
#22791 = DIRECTION ( 'NONE',  ( -1.000000000000000000, 0.000000000000000000, 0.000000000000000000 ) ) ;
#22792 = PRESENTATION_STYLE_ASSIGNMENT (( #16873 ) ) ;
#22793 = VERTEX_POINT ( 'NONE', #22622 ) ;
#22794 = DIRECTION ( 'NONE',  ( 0.000000000000000000, -1.000000000000000000, 2.999999999999999839E-15 ) ) ;
#22795 = CARTESIAN_POINT ( 'NONE',  ( 29.81606138205706458, -34.54722833698622964, 70.28164373264664277 ) ) ;
#22796 = CARTESIAN_POINT ( 'NONE',  ( 40.26954217208372455, 1.096159133578081812, 72.86986841596736042 ) ) ;
#22797 = ORIENTED_EDGE ( 'NONE', *, *, #20190, .T. ) ;
#22798 = DIRECTION ( 'NONE',  ( 2.690219486203388234E-15, -0.8967398287344627850, -0.4425581086832399147 ) ) ;
#22799 = CARTESIAN_POINT ( 'NONE',  ( 31.01606138205699992, 2.823374736507280597E-13, 81.37823623207336254 ) ) ;
#22800 = CARTESIAN_POINT ( 'NONE',  ( 39.75915168707250302, -0.7136820888860997414, 70.26145752964252722 ) ) ;
#22801 = CARTESIAN_POINT ( 'NONE',  ( 45.81606138205700063, 44.92314894770294131, 80.37823623207322044 ) ) ;
#22802 = CARTESIAN_POINT ( 'NONE',  ( 39.38009889167650357, -20.21368208888610951, 72.75271321436731853 ) ) ;
#22803 = VECTOR ( 'NONE', #13450, 1000.000000000000000 ) ;
#22804 = DIRECTION ( 'NONE',  ( 0.000000000000000000, 1.000000000000000000, -6.938893903907222067E-15 ) ) ;
#22805 = CIRCLE ( 'NONE', #14991, 1.499999999999999778 ) ;
#22806 = CARTESIAN_POINT ( 'NONE',  ( 33.81606138205700063, 15.19123852234700323, 70.30501292736995822 ) ) ;
#22807 = EDGE_CURVE ( 'NONE', #2274, #3431, #15019, .T. ) ;
#22808 = CARTESIAN_POINT ( 'NONE',  ( 38.93987200065210175, -18.80384086642191122, 72.33091598616826445 ) ) ;
#22809 = CARTESIAN_POINT ( 'NONE',  ( 39.38009889167650357, -6.213682088886108623, 72.75271321436733274 ) ) ;
#22810 = EDGE_CURVE ( 'NONE', #15469, #10773, #14513, .T. ) ;
#22811 = ORIENTED_EDGE ( 'NONE', *, *, #4401, .F. ) ;
#22812 = DIRECTION ( 'NONE',  ( 0.000000000000000000, 1.000000000000000000, 0.000000000000000000 ) ) ;
#22813 = ORIENTED_EDGE ( 'NONE', *, *, #7374, .F. ) ;
#22814 = CARTESIAN_POINT ( 'NONE',  ( 39.95015449827720744, -7.003840866421910505, 71.96809898377888715 ) ) ;
#22815 = DIRECTION ( 'NONE',  ( -1.734723475976814737E-16, 1.000000000000000000, -3.491481338843135327E-15 ) ) ;
#22816 = EDGE_CURVE ( 'NONE', #23642, #18207, #21781, .T. ) ;
#22817 = CARTESIAN_POINT ( 'NONE',  ( 37.33957961208646736, 0.1863179111138910105, 72.81632618279323310 ) ) ;
#22818 = VERTEX_POINT ( 'NONE', #12476 ) ;
#22819 = CARTESIAN_POINT ( 'NONE',  ( 39.64521430340304420, -8.813682088886096722, 69.45876917294177133 ) ) ;
#22820 = VERTEX_POINT ( 'NONE', #14636 ) ;
#22821 = DIRECTION ( 'NONE',  ( -1.000000000000000000, 0.000000000000000000, 0.000000000000000000 ) ) ;
#22822 = AXIS2_PLACEMENT_3D ( 'NONE', #12551, #18208, #20387 ) ;
#22823 = CARTESIAN_POINT ( 'NONE',  ( 37.60469502381300799, -12.40384086642191441, 72.26730301774234988 ) ) ;
#22824 = DIRECTION ( 'NONE',  ( -3.717264591378870232E-16, -2.999999999999999839E-15, -1.000000000000000000 ) ) ;
#22825 = VERTEX_POINT ( 'NONE', #22493 ) ;
#22826 = DIRECTION ( 'NONE',  ( 0.000000000000000000, 1.000000000000000000, -2.913263826201159484E-15 ) ) ;
#22827 = LINE ( 'NONE', #12671, #15337 ) ;
#22828 = CARTESIAN_POINT ( 'NONE',  ( 35.86008812008917346, -18.10384086642191548, 71.32335560751961623 ) ) ;
#22829 = CARTESIAN_POINT ( 'NONE',  ( 37.79585267494195477, -22.15691033384591080, 75.30013673462515555 ) ) ;
#22830 = CARTESIAN_POINT ( 'NONE',  ( 39.29254315202756231, -22.81368208888610027, 69.94417936956672577 ) ) ;
#22831 = DIRECTION ( 'NONE',  ( 0.000000000000000000, -0.6595716529892415858, 0.7516416929448761497 ) ) ;
#22832 = ADVANCED_FACE ( 'NONE', ( #18890 ), #20697, .F. ) ;
#22833 = CARTESIAN_POINT ( 'NONE',  ( 35.31606138205687273, 42.19123852234596939, 65.30501292736988717 ) ) ;
#22834 = ORIENTED_EDGE ( 'NONE', *, *, #20364, .T. ) ;
#22835 = CARTESIAN_POINT ( 'NONE',  ( 41.31606138205700063, 3.392460599465057403, 64.84545171350526971 ) ) ;
#22836 = CARTESIAN_POINT ( 'NONE',  ( 40.31606138205700773, -29.30876147765401640, 69.30501292737010033 ) ) ;
#22837 = CARTESIAN_POINT ( 'NONE',  ( 40.14115730948191185, -11.10384086642191015, 71.43714994484034264 ) ) ;
#22838 = AXIS2_PLACEMENT_3D ( 'NONE', #21653, #7628, #23194 ) ;
#22839 = SHAPE_DEFINITION_REPRESENTATION ( #17538, #14684 ) ;
#22840 = DIRECTION ( 'NONE',  ( 1.445602896647340149E-16, -0.8212051873014210024, -0.5706330172266920187 ) ) ;
#22841 = CARTESIAN_POINT ( 'NONE',  ( 37.80618814713140097, -25.91368208888610880, 73.13360434286902034 ) ) ;
#22842 = CARTESIAN_POINT ( 'NONE',  ( 44.81606138205700063, 28.12806996228107081, 65.30501292736992980 ) ) ;
#22843 = CARTESIAN_POINT ( 'NONE',  ( 36.49096545463212493, -24.10384086642190482, 71.32335560751960202 ) ) ;
#22844 = CARTESIAN_POINT ( 'NONE',  ( 36.51585873400316018, -6.269825903680327883, 82.74874648979978531 ) ) ;
#22845 = CARTESIAN_POINT ( 'NONE',  ( 38.82593461698262871, -26.91368208888610170, 69.62690120949091011 ) ) ;
#22846 = ORIENTED_EDGE ( 'NONE', *, *, #4479, .T. ) ;
#22847 = ORIENTED_EDGE ( 'NONE', *, *, #6786, .T. ) ;
#22848 = DIRECTION ( 'NONE',  ( 0.000000000000000000, 0.8967398287344625629, 0.4425581086832402478 ) ) ;
#22849 = PLANE ( 'NONE',  #17466 ) ;
#22850 = CARTESIAN_POINT ( 'NONE',  ( 37.38336156205274818, 0.2863179111139008137, 72.12822762946751709 ) ) ;
#22851 = ORIENTED_EDGE ( 'NONE', *, *, #21393, .T. ) ;
#22852 = ORIENTED_EDGE ( 'NONE', *, *, #24963, .F. ) ;
#22853 = DIRECTION ( 'NONE',  ( 1.000000000000000000, 2.999999999999999839E-15, 0.000000000000000000 ) ) ;
#22854 = DIRECTION ( 'NONE',  ( 0.000000000000000000, -0.5706330172266915746, 0.8212051873014213355 ) ) ;
#22855 = ORIENTED_EDGE ( 'NONE', *, *, #7895, .T. ) ;
#22856 = DIRECTION ( 'NONE',  ( 0.000000000000000000, -0.3299742535180969494, 0.9439899321577399638 ) ) ;
#22857 = CARTESIAN_POINT ( 'NONE',  ( 36.68196826583682935, -2.003840866421909617, 70.79240656858108593 ) ) ;
#22858 = EDGE_CURVE ( 'NONE', #14577, #4754, #8857, .T. ) ;
#22859 = EDGE_CURVE ( 'NONE', #15969, #24147, #2897, .T. ) ;
#22860 = FACE_OUTER_BOUND ( 'NONE', #5455, .T. ) ;
#22861 = ADVANCED_FACE ( 'NONE', ( #8728 ), #18631, .T. ) ;
#22862 = DIRECTION ( 'NONE',  ( -1.000000000000000000, 0.000000000000000000, 0.000000000000000000 ) ) ;
#22863 = ORIENTED_EDGE ( 'NONE', *, *, #16265, .F. ) ;
#22864 = ORIENTED_EDGE ( 'NONE', *, *, #19782, .T. ) ;
#22865 = ORIENTED_EDGE ( 'NONE', *, *, #20276, .T. ) ;
#22866 = CYLINDRICAL_SURFACE ( 'NONE', #6717, 1.500000000000001332 ) ;
#22867 = CARTESIAN_POINT ( 'NONE',  ( 37.25202387243752611, -1.213682088886100630, 70.00779233799264034 ) ) ;
#22868 = CARTESIAN_POINT ( 'NONE',  ( 38.26194895904384907, -28.60384086642191548, 73.11602215082115208 ) ) ;
#22869 =( NAMED_UNIT ( * ) PLANE_ANGLE_UNIT ( ) SI_UNIT ( $, .RADIAN. ) );
#22870 = DIRECTION ( 'NONE',  ( 1.000000000000000000, 1.734723475976804876E-16, -1.734723475976814737E-16 ) ) ;
#22871 = VERTEX_POINT ( 'NONE', #12720 ) ;
#22872 = LINE ( 'NONE', #5230, #11052 ) ;
#22873 = EDGE_CURVE ( 'NONE', #13029, #13874, #11941, .T. ) ;
#22874 = CARTESIAN_POINT ( 'NONE',  ( 31.81606138205700418, -21.15876147765404625, 76.30501292736998664 ) ) ;
#22875 = DIRECTION ( 'NONE',  ( 0.000000000000000000, 3.469446951953613400E-15, 1.000000000000000000 ) ) ;
#22876 = CARTESIAN_POINT ( 'NONE',  ( 38.31606138205700063, -0.7263636227174442572, 61.39059882987834982 ) ) ;
#22877 = SURFACE_SIDE_STYLE ('',( #11169 ) ) ;
#22878 = DIRECTION ( 'NONE',  ( 0.000000000000000000, 1.163336342344335610E-15, -1.000000000000000000 ) ) ;
#22879 = VERTEX_POINT ( 'NONE', #16434 ) ;
#22880 = ORIENTED_EDGE ( 'NONE', *, *, #3075, .T. ) ;
#22881 = LINE ( 'NONE', #16703, #2131 ) ;
#22882 = CARTESIAN_POINT ( 'NONE',  ( 44.81606138205700063, -21.15876147765404625, 76.30501292736998664 ) ) ;
#22883 = CARTESIAN_POINT ( 'NONE',  ( 37.25260217561390874, -17.61368208888609743, 71.78268878715392987 ) ) ;
#22884 = ORIENTED_EDGE ( 'NONE', *, *, #19484, .F. ) ;
#22885 = VERTEX_POINT ( 'NONE', #969 ) ;
#22886 = CARTESIAN_POINT ( 'NONE',  ( 29.81606138205706458, -34.54722833698622964, 70.28164373264664277 ) ) ;
#22887 = CARTESIAN_POINT ( 'NONE',  ( 38.26194895904383486, 0.9863179111138999922, 69.64448340153880679 ) ) ;
#22888 = CARTESIAN_POINT ( 'NONE',  ( 38.82593461698265003, -20.70384086642191335, 73.13360434286903455 ) ) ;
#22889 = DIRECTION ( 'NONE',  ( 0.000000000000000000, -0.9992330079037401447, 0.03915859951075795903 ) ) ;
#22890 = CARTESIAN_POINT ( 'NONE',  ( 35.86008812008917346, -3.513682088886104005, 71.43714994484035685 ) ) ;
#22891 = CARTESIAN_POINT ( 'NONE',  ( 33.31606138205700773, 7.043113989679085307, 66.83274420321491505 ) ) ;
#22892 = CARTESIAN_POINT ( 'NONE',  ( 39.91050633825327054, -5.989745541782124150, 83.27615889399532989 ) ) ;
#22893 = DIRECTION ( 'NONE',  ( 0.000000000000000000, 0.4425581086832400257, -0.8967398287344627850 ) ) ;
#22894 = CARTESIAN_POINT ( 'NONE',  ( 30.81606138205700418, 40.39281886181299797, 80.75501292736983316 ) ) ;
#22895 = CARTESIAN_POINT ( 'NONE',  ( 38.31606138205700063, 38.69123852234599781, 75.30501292737004349 ) ) ;
#22896 = CARTESIAN_POINT ( 'NONE',  ( 31.81606138205700418, -26.97987052895604876, 80.55501292737007191 ) ) ;
#22897 = EDGE_CURVE ( 'NONE', #5254, #7327, #24790, .T. ) ;
#22898 = DIRECTION ( 'NONE',  ( 1.000000000000000000, -1.115179377413661005E-30, -3.717264591378870232E-16 ) ) ;
#22899 = VECTOR ( 'NONE', #21697, 1000.000000000000000 ) ;
#22900 = VECTOR ( 'NONE', #20122, 1000.000000000000000 ) ;
#22901 = VERTEX_POINT ( 'NONE', #6787 ) ;
#22902 = CYLINDRICAL_SURFACE ( 'NONE', #378, 2.000000000000001776 ) ;
#22903 = DIRECTION ( 'NONE',  ( 0.000000000000000000, 0.4425581086832397482, -0.8967398287344628960 ) ) ;
#22904 = ORIENTED_EDGE ( 'NONE', *, *, #2938, .F. ) ;
#22905 = ORIENTED_EDGE ( 'NONE', *, *, #24961, .T. ) ;
#22906 = PRODUCT_DEFINITION_CONTEXT ( 'detailed design', #19335, 'design' ) ;
#22907 = CARTESIAN_POINT ( 'NONE',  ( 36.07789103942399578, -8.203840866421915123, 72.05058123536544201 ) ) ;
#22908 = CARTESIAN_POINT ( 'NONE',  ( 44.06606138205700063, 42.82479937715250173, 82.59790614618330551 ) ) ;
#22909 = CARTESIAN_POINT ( 'NONE',  ( 36.80608444377001121, -23.31368208888610383, 70.35351908239857721 ) ) ;
#22910 =( NAMED_UNIT ( * ) PLANE_ANGLE_UNIT ( ) SI_UNIT ( $, .RADIAN. ) );
#22911 = VERTEX_POINT ( 'NONE', #12601 ) ;
#22912 = DIRECTION ( 'NONE',  ( 0.000000000000000000, 0.000000000000000000, -1.000000000000000000 ) ) ;
#22913 = CARTESIAN_POINT ( 'NONE',  ( 29.81606138205705037, -30.46100403034036219, 72.05704881431053366 ) ) ;
#22914 = CARTESIAN_POINT ( 'NONE',  ( 40.55423172469004811, -20.41368208888610880, 72.05058123536544201 ) ) ;
#22915 = ORIENTED_EDGE ( 'NONE', *, *, #12266, .T. ) ;
#22916 = LINE ( 'NONE', #1143, #25447 ) ;
#22917 = VECTOR ( 'NONE', #21281, 1000.000000000000114 ) ;
#22918 = VECTOR ( 'NONE', #14074, 1000.000000000000000 ) ;
#22919 = CARTESIAN_POINT ( 'NONE',  ( 38.37017380507020192, -4.013682088886107557, 73.11602215082118050 ) ) ;
#22920 = DIRECTION ( 'NONE',  ( -1.000000000000000000, 0.000000000000000000, 0.000000000000000000 ) ) ;
#22921 = CARTESIAN_POINT ( 'NONE',  ( 39.95015449827720744, -14.61368208888610454, 70.79240656858105751 ) ) ;
#22922 = LINE ( 'NONE', #17526, #1991 ) ;
#22923 = EDGE_CURVE ( 'NONE', #7089, #18567, #14764, .T. ) ;
#22924 = DIRECTION ( 'NONE',  ( 5.664403186863039509E-16, 3.000000000000000628E-15, 1.000000000000000000 ) ) ;
#22925 = CARTESIAN_POINT ( 'NONE',  ( 39.31564783533279694, -21.30384086642190766, 70.72433947564853440 ) ) ;
#22926 = CARTESIAN_POINT ( 'NONE',  ( 39.95015449827720744, -8.613682088886104538, 70.79240656858107172 ) ) ;
#22927 = EDGE_LOOP ( 'NONE', ( #25109, #6922, #23673, #3663, #3403, #18001, #24097, #1655, #11022, #9280, #7287, #9634 ) ) ;
#22928 = CARTESIAN_POINT ( 'NONE',  ( 35.81606138205700063, 5.191238522346999673, 69.30501292736998664 ) ) ;
#22929 = ORIENTED_EDGE ( 'NONE', *, *, #19961, .F. ) ;
#22930 = ORIENTED_EDGE ( 'NONE', *, *, #18309, .F. ) ;
#22931 = CARTESIAN_POINT ( 'NONE',  ( 39.98359781491296161, -5.203840866421911571, 70.89533451361947414 ) ) ;
#22932 = DIRECTION ( 'NONE',  ( 4.341746501209495972E-16, -0.4341746501209495790, -0.9008287146801833289 ) ) ;
#22933 = VECTOR ( 'NONE', #9350, 1000.000000000000000 ) ;
#22934 = VECTOR ( 'NONE', #3183, 1000.000000000000114 ) ;
#22935 = CARTESIAN_POINT ( 'NONE',  ( 40.14115730948191185, 1.486317911113896884, 71.32335560751963044 ) ) ;
#22936 = ORIENTED_EDGE ( 'NONE', *, *, #20684, .T. ) ;
#22937 = CARTESIAN_POINT ( 'NONE',  ( 40.77203464402485622, -6.513682088886103116, 71.32335560751961623 ) ) ;
#22938 = ORIENTED_EDGE ( 'NONE', *, *, #14297, .F. ) ;
#22939 = CARTESIAN_POINT ( 'NONE',  ( 29.81606138205707168, -36.31746077171918330, 73.86860304758450013 ) ) ;
#22940 = CARTESIAN_POINT ( 'NONE',  ( 39.02742774030101458, -5.403840866421909972, 70.49320253461759478 ) ) ;
#22941 = EDGE_CURVE ( 'NONE', #11458, #17655, #16698, .T. ) ;
#22942 = LINE ( 'NONE', #19589, #18010 ) ;
#22943 = EDGE_CURVE ( 'NONE', #3712, #17085, #10780, .T. ) ;
#22944 = ORIENTED_EDGE ( 'NONE', *, *, #15712, .T. ) ;
#22945 = CARTESIAN_POINT ( 'NONE',  ( 44.81606138205700063, 35.44123852234597649, 68.80501292736990138 ) ) ;
#22946 = FACE_OUTER_BOUND ( 'NONE', #18587, .T. ) ;
#22947 = CARTESIAN_POINT ( 'NONE',  ( 39.02088643472237806, -18.70384086642192045, 73.73360434286898624 ) ) ;
#22948 = EDGE_CURVE ( 'NONE', #13145, #24731, #7035, .T. ) ;
#22949 = EDGE_CURVE ( 'NONE', #15873, #22756, #16955, .T. ) ;
#22950 = EDGE_CURVE ( 'NONE', #9537, #821, #12976, .T. ) ;
#22951 = CARTESIAN_POINT ( 'NONE',  ( 37.31068429205632953, -21.95512953228131892, 75.30323118459136822 ) ) ;
#22952 = SURFACE_SIDE_STYLE ('',( #3373 ) ) ;
#22953 = CARTESIAN_POINT ( 'NONE',  ( 38.37017380507020192, -18.01368208888611022, 73.11602215082116629 ) ) ;
#22954 = LINE ( 'NONE', #13308, #25271 ) ;
#22955 = DIRECTION ( 'NONE',  ( 0.000000000000000000, -3.469446951953613400E-15, -1.000000000000000000 ) ) ;
#22956 = AXIS2_PLACEMENT_3D ( 'NONE', #12092, #13885, #2399 ) ;
#22957 = ORIENTED_EDGE ( 'NONE', *, *, #5010, .T. ) ;
#22958 = VECTOR ( 'NONE', #5262, 1000.000000000000000 ) ;
#22959 = CARTESIAN_POINT ( 'NONE',  ( 36.81606138205700063, -6.758471399387619094, 56.13572720721855092 ) ) ;
#22960 = CARTESIAN_POINT ( 'NONE',  ( 36.06606138205700063, 5.594015759443068170, 2.006005027196319901 ) ) ;
#22961 = ADVANCED_FACE ( 'NONE', ( #9117, #5232, #9364 ), #11551, .T. ) ;
#22962 = CARTESIAN_POINT ( 'NONE',  ( 36.64852494920107517, -8.203840866421909794, 71.86517103874049894 ) ) ;
#22963 = ADVANCED_FACE ( 'NONE', ( #19144 ), #13216, .T. ) ;
#22964 = CARTESIAN_POINT ( 'NONE',  ( 43.81606138205700063, 2.191238522347000117, 69.30501292737000085 ) ) ;
#22965 = CARTESIAN_POINT ( 'NONE',  ( 37.33957961208646736, -25.81368208888610738, 72.81632618279320468 ) ) ;
#22966 = CARTESIAN_POINT ( 'NONE',  ( 43.31606138205700063, 3.296535697557910538, 65.33616386252352015 ) ) ;
#22967 = CARTESIAN_POINT ( 'NONE',  ( 36.49096545463212493, -26.10384086642190482, 71.32335560751960202 ) ) ;
#22968 = CARTESIAN_POINT ( 'NONE',  ( 36.31606138205700063, -7.204193249396275256, 83.11277699141410835 ) ) ;
#22969 = CARTESIAN_POINT ( 'NONE',  ( 37.25202387243752611, -17.21368208888610241, 70.00779233799262613 ) ) ;
#22970 = ORIENTED_EDGE ( 'NONE', *, *, #15892, .F. ) ;
#22971 = CARTESIAN_POINT ( 'NONE',  ( 36.98690846071097837, -25.81368208888611093, 73.30173637941817333 ) ) ;
#22972 = ORIENTED_EDGE ( 'NONE', *, *, #14747, .T. ) ;
#22973 = FACE_OUTER_BOUND ( 'NONE', #4960, .T. ) ;
#22974 = CARTESIAN_POINT ( 'NONE',  ( 43.31606138205700773, -19.47805968271054766, 24.94720442500192448 ) ) ;
#22975 = CARTESIAN_POINT ( 'NONE',  ( 38.37017380507020192, 1.986317911113897550, 72.51602215082118619 ) ) ;
#22976 = CIRCLE ( 'NONE', #12700, 1.750000000000001776 ) ;
#22977 = ORIENTED_EDGE ( 'NONE', *, *, #2467, .T. ) ;
#22978 = ORIENTED_EDGE ( 'NONE', *, *, #18074, .T. ) ;
#22979 = DIRECTION ( 'NONE',  ( 0.000000000000000000, 1.000000000000000000, 0.000000000000000000 ) ) ;
#22980 = CYLINDRICAL_SURFACE ( 'NONE', #8348, 0.7500000000000008882 ) ;
#22981 = VERTEX_POINT ( 'NONE', #11679 ) ;
#22982 = CARTESIAN_POINT ( 'NONE',  ( 40.14115730948191185, -3.103840866421910150, 71.43714994484034264 ) ) ;
#22983 = VECTOR ( 'NONE', #12238, 1000.000000000000000 ) ;
#22984 = DIRECTION ( 'NONE',  ( 1.000000000000000000, 0.000000000000000000, 0.000000000000000000 ) ) ;
#22985 = DIRECTION ( 'NONE',  ( 1.000000000000000000, 2.999999999999999839E-15, 0.000000000000000000 ) ) ;
#22986 = ORIENTED_EDGE ( 'NONE', *, *, #10810, .T. ) ;
#22987 = STYLED_ITEM ( 'NONE', ( #25279 ), #25350 ) ;
#22988 = CARTESIAN_POINT ( 'NONE',  ( 35.81606138205700063, 37.44123852234599781, 75.30501292736990138 ) ) ;
#22989 = CARTESIAN_POINT ( 'NONE',  ( 38.26194895904383486, 0.9863179111138999922, 69.64448340153880679 ) ) ;
#22990 = VERTEX_POINT ( 'NONE', #9489 ) ;
#22991 = CARTESIAN_POINT ( 'NONE',  ( 39.29254315202757653, -28.80384086642191832, 72.81632618279320468 ) ) ;
#22992 = DIRECTION ( 'NONE',  ( 0.000000000000000000, 3.469446951953611033E-15, 1.000000000000000000 ) ) ;
#22993 = VECTOR ( 'NONE', #6376, 1000.000000000000000 ) ;
#22994 = ORIENTED_EDGE ( 'NONE', *, *, #15098, .F. ) ;
#22995 = DIRECTION ( 'NONE',  ( 1.000000000000000000, 0.000000000000000000, 0.000000000000000000 ) ) ;
#22996 = EDGE_CURVE ( 'NONE', #19039, #23539, #3424, .T. ) ;
#22997 = DIRECTION ( 'NONE',  ( 0.000000000000000000, -1.000000000000000000, 0.000000000000000000 ) ) ;
#22998 = PLANE ( 'NONE',  #3565 ) ;
#22999 = CIRCLE ( 'NONE', #14783, 0.4999999999999982792 ) ;
#23000 = ORIENTED_EDGE ( 'NONE', *, *, #17938, .F. ) ;
#23001 = PRODUCT_DEFINITION ( 'UNKNOWN', '', #2235, #20856 ) ;
#23002 = CARTESIAN_POINT ( 'NONE',  ( 44.06606138205700063, 41.63025572888945192, 83.79244979444629848 ) ) ;
#23003 = ORIENTED_EDGE ( 'NONE', *, *, #7202, .F. ) ;
#23004 = ORIENTED_EDGE ( 'NONE', *, *, #20684, .F. ) ;
#23005 = CARTESIAN_POINT ( 'NONE',  ( 36.31606138205700063, 39.69123852234599070, 73.55501292736988717 ) ) ;
#23006 = VECTOR ( 'NONE', #3062, 1000.000000000000000 ) ;
#23007 = CARTESIAN_POINT ( 'NONE',  ( 38.44255644662678861, -39.60718113818700203, 84.30501292737011454 ) ) ;
#23008 = CARTESIAN_POINT ( 'NONE',  ( 37.21915885897815457, -19.41368208888609814, 71.08074471024443142 ) ) ;
#23009 = ORIENTED_EDGE ( 'NONE', *, *, #16629, .T. ) ;
#23010 = ORIENTED_EDGE ( 'NONE', *, *, #10782, .F. ) ;
#23011 = DIRECTION ( 'NONE',  ( 1.000000000000000000, 2.611101091812726599E-15, -1.919289851541777660E-16 ) ) ;
#23012 = DIRECTION ( 'NONE',  ( -4.625929269271484533E-15, 0.8967398287344634511, 0.4425581086832385824 ) ) ;
#23013 = CARTESIAN_POINT ( 'NONE',  ( 37.33957961208645315, -23.80384086642191122, 69.94417936956671156 ) ) ;
#23014 = VECTOR ( 'NONE', #19478, 1000.000000000000000 ) ;
#23015 = LINE ( 'NONE', #13247, #16117 ) ;
#23016 = VECTOR ( 'NONE', #12697, 1000.000000000000000 ) ;
#23017 = ORIENTED_EDGE ( 'NONE', *, *, #14150, .F. ) ;
#23018 = CARTESIAN_POINT ( 'NONE',  ( 43.38751330861538236, 3.099072278389038981, 6.135933108610800879 ) ) ;
#23019 = CARTESIAN_POINT ( 'NONE',  ( 43.31606138205700063, -16.77230293220685198, 77.52306850662458260 ) ) ;
#23020 = DIRECTION ( 'NONE',  ( 8.967398287344632705E-16, -0.8967398287344631180, -0.4425581086832391375 ) ) ;
#23021 = VECTOR ( 'NONE', #837, 1000.000000000000000 ) ;
#23022 = CARTESIAN_POINT ( 'NONE',  ( 40.21566563214662438, -6.564967302039574903, 83.21717579561996558 ) ) ;
#23023 = LINE ( 'NONE', #19413, #15548 ) ;
#23024 = ADVANCED_FACE ( 'NONE', ( #23247 ), #7552, .T. ) ;
#23025 = DIRECTION ( 'NONE',  ( 0.000000000000000000, -1.000000000000000000, 0.000000000000000000 ) ) ;
#23026 = ADVANCED_FACE ( 'NONE', ( #23118 ), #3293, .T. ) ;
#23027 = ORIENTED_EDGE ( 'NONE', *, *, #21829, .T. ) ;
#23028 = LINE ( 'NONE', #18663, #22612 ) ;
#23029 = CARTESIAN_POINT ( 'NONE',  ( 41.14099152588523367, -10.60718113818700026, 93.30501292736998664 ) ) ;
#23030 = ORIENTED_EDGE ( 'NONE', *, *, #1756, .F. ) ;
#23031 = ORIENTED_EDGE ( 'NONE', *, *, #19250, .T. ) ;
#23032 = CARTESIAN_POINT ( 'NONE',  ( 36.36258059203030513, -13.90384086642191264, 69.89063713639259845 ) ) ;
#23033 = VECTOR ( 'NONE', #17942, 1000.000000000000000 ) ;
#23034 = CIRCLE ( 'NONE', #12777, 1.000000000000000888 ) ;
#23035 = CARTESIAN_POINT ( 'NONE',  ( 42.74055771317608787, 3.188265934946779012, 6.371314334530746137 ) ) ;
#23036 = CARTESIAN_POINT ( 'NONE',  ( 36.87297107704152666, -13.71368208888610773, 72.49904802271740323 ) ) ;
#23037 = VECTOR ( 'NONE', #23183, 1000.000000000000000 ) ;
#23038 = VERTEX_POINT ( 'NONE', #15402 ) ;
#23039 = LINE ( 'NONE', #21365, #12175 ) ;
#23040 = DIRECTION ( 'NONE',  ( 0.000000000000000000, -1.000000000000000000, 2.999999999999999839E-15 ) ) ;
#23041 = EDGE_CURVE ( 'NONE', #5522, #10597, #15650, .T. ) ;
#23042 = CARTESIAN_POINT ( 'NONE',  ( 36.07789103942398867, -19.41368208888610525, 70.70992431699450265 ) ) ;
#23043 = ORIENTED_EDGE ( 'NONE', *, *, #24963, .T. ) ;
#23044 = DIRECTION ( 'NONE',  ( 1.000000000000000000, 2.999999999999999839E-15, 0.000000000000000000 ) ) ;
#23045 = CARTESIAN_POINT ( 'NONE',  ( 40.64099152588522657, -1.357181138186998925, 79.30501292737000085 ) ) ;
#23046 = DIRECTION ( 'NONE',  ( 1.000000000000000000, 2.999999999999999839E-15, 0.000000000000000000 ) ) ;
#23047 = AXIS2_PLACEMENT_3D ( 'NONE', #1039, #22821, #17032 ) ;
#23048 = DIRECTION ( 'NONE',  ( 3.469446951953614189E-15, -0.8967398287344635621, -0.4425581086832386379 ) ) ;
#23049 = CARTESIAN_POINT ( 'NONE',  ( 36.51585873400316018, -6.323107536394523720, 83.24593316792127951 ) ) ;
#23050 = CIRCLE ( 'NONE', #9488, 2.500000000000002220 ) ;
#23051 = CARTESIAN_POINT ( 'NONE',  ( 38.26194895904384197, -12.60384086642191015, 72.51602215082118619 ) ) ;
#23052 = CARTESIAN_POINT ( 'NONE',  ( 36.80608444377001121, 0.6863179111138983934, 70.35351908239860563 ) ) ;
#23053 = ORIENTED_EDGE ( 'NONE', *, *, #15120, .F. ) ;
#23054 = CARTESIAN_POINT ( 'NONE',  ( 29.71606138205697434, -29.47337283097074234, 44.07055847651732705 ) ) ;
#23055 = CARTESIAN_POINT ( 'NONE',  ( 35.31606138205700773, 7.535758204303438568, 66.26723409915207696 ) ) ;
#23056 = ORIENTED_EDGE ( 'NONE', *, *, #3773, .T. ) ;
#23057 = ORIENTED_EDGE ( 'NONE', *, *, #16568, .F. ) ;
#23058 = CARTESIAN_POINT ( 'NONE',  ( 37.80618814713138676, 0.2961591335780937584, 69.62690120949091011 ) ) ;
#23059 = CARTESIAN_POINT ( 'NONE',  ( 38.26194895904383486, -29.01368208888610312, 70.24448340153875847 ) ) ;
#23060 = PRODUCT_DEFINITION_SHAPE ( 'NONE', 'NONE',  #21901 ) ;
#23061 = CARTESIAN_POINT ( 'NONE',  ( 37.61123632939165873, -11.91368208888610880, 73.73360434286898624 ) ) ;
#23062 = EDGE_LOOP ( 'NONE', ( #11004, #1952, #10128, #9876 ) ) ;
#23063 = CYLINDRICAL_SURFACE ( 'NONE', #11547, 2.500000000000002220 ) ;
#23064 = CARTESIAN_POINT ( 'NONE',  ( 38.63098279924290068, -6.703840866421912459, 72.53360434286905445 ) ) ;
#23065 = DIRECTION ( 'NONE',  ( 0.000000000000000000, 2.999999999999999839E-15, 1.000000000000000000 ) ) ;
#23066 = AXIS2_PLACEMENT_3D ( 'NONE', #3809, #2256, #19786 ) ;
#23067 = ORIENTED_EDGE ( 'NONE', *, *, #11473, .F. ) ;
#23068 = PLANE ( 'NONE',  #600 ) ;
#23069 = DIRECTION ( 'NONE',  ( 0.000000000000000000, -2.999999999999999839E-15, -1.000000000000000000 ) ) ;
#23070 = CARTESIAN_POINT ( 'NONE',  ( 38.26194895904384197, -10.60384086642192081, 73.71602215082116061 ) ) ;
#23071 = VECTOR ( 'NONE', #4731, 1000.000000000000114 ) ;
#23072 = CARTESIAN_POINT ( 'NONE',  ( 36.31606138205700063, -20.35127826328909251, 75.48051798356576114 ) ) ;
#23073 = SURFACE_SIDE_STYLE ('',( #10738 ) ) ;
#23074 = CARTESIAN_POINT ( 'NONE',  ( 37.80618814713140097, -13.91368208888610347, 73.13360434286903455 ) ) ;
#23075 = CARTESIAN_POINT ( 'NONE',  ( 40.64099152588522657, -1.357181138186998925, 80.05501292737000085 ) ) ;
#23076 = DIRECTION ( 'NONE',  ( 1.000000000000000000, 0.000000000000000000, 0.000000000000000000 ) ) ;
#23077 = ORIENTED_EDGE ( 'NONE', *, *, #20096, .T. ) ;
#23078 = CYLINDRICAL_SURFACE ( 'NONE', #11838, 0.4999999999999982792 ) ;
#23079 = CARTESIAN_POINT ( 'NONE',  ( 38.93415946300897446, -11.50384086642190518, 69.66206559358664663 ) ) ;
#23080 = SHAPE_DEFINITION_REPRESENTATION ( #11581, #10266 ) ;
#23081 = DIRECTION ( 'NONE',  ( 0.000000000000000000, -1.000000000000000000, 3.491481338843135327E-15 ) ) ;
#23082 = ADVANCED_FACE ( 'NONE', ( #21201 ), #17213, .T. ) ;
#23083 = CARTESIAN_POINT ( 'NONE',  ( 39.29254315202756231, -24.81368208888610383, 69.94417936956671156 ) ) ;
#23084 = ADVANCED_FACE ( 'NONE', ( #25297 ), #19386, .T. ) ;
#23085 = CARTESIAN_POINT ( 'NONE',  ( 33.31606138205700773, 3.392460599465057403, 64.84545171350526971 ) ) ;
#23086 = EDGE_CURVE ( 'NONE', #12767, #23547, #18317, .T. ) ;
#23087 = CIRCLE ( 'NONE', #20212, 1.500000000000001332 ) ;
#23088 = EDGE_CURVE ( 'NONE', #6472, #10846, #1358, .T. ) ;
#23089 = CARTESIAN_POINT ( 'NONE',  ( 36.80608444377001831, -20.30384086642191477, 72.40698646996135324 ) ) ;
#23090 = EDGE_CURVE ( 'NONE', #24103, #22354, #21320, .T. ) ;
#23091 = CARTESIAN_POINT ( 'NONE',  ( 36.51585873400316018, -6.323107536394523720, 83.24593316792127951 ) ) ;
#23092 = MECHANICAL_DESIGN_GEOMETRIC_PRESENTATION_REPRESENTATION (  '', ( #16512 ), #21048 ) ;
#23093 = CARTESIAN_POINT ( 'NONE',  ( 36.68196826583682935, -17.61368208888610454, 71.96809898377888715 ) ) ;
#23094 = ORIENTED_EDGE ( 'NONE', *, *, #15663, .T. ) ;
#23095 = CARTESIAN_POINT ( 'NONE',  ( 36.89935272106205133, -0.4038408664219194089, 73.23812341099225875 ) ) ;
#23096 = ORIENTED_EDGE ( 'NONE', *, *, #20754, .T. ) ;
#23097 = CARTESIAN_POINT ( 'NONE',  ( 42.06606138205700063, 42.19123852234599781, 75.30501292736987295 ) ) ;
#23098 = DIRECTION ( 'NONE',  ( 0.000000000000000000, -3.469446951953611033E-15, 1.000000000000000000 ) ) ;
#23099 = CARTESIAN_POINT ( 'NONE',  ( 39.31564783533279694, -23.30384086642191477, 70.72433947564853440 ) ) ;
#23100 = ORIENTED_EDGE ( 'NONE', *, *, #24135, .F. ) ;
#23101 = ORIENTED_EDGE ( 'NONE', *, *, #12417, .F. ) ;
#23102 = PLANE ( 'NONE',  #7187 ) ;
#23103 = DIRECTION ( 'NONE',  ( 0.000000000000000000, -0.5735764363510444941, 0.8191520442889929088 ) ) ;
#23104 = CARTESIAN_POINT ( 'NONE',  ( 38.31606138205700063, 42.51966564709218943, 72.30501292737018559 ) ) ;
#23105 = CARTESIAN_POINT ( 'NONE',  ( 39.12911128074872380, -27.50384086642191406, 69.06206559358663810 ) ) ;
#23106 = EDGE_CURVE ( 'NONE', #1156, #9497, #9621, .T. ) ;
#23107 = CARTESIAN_POINT ( 'NONE',  ( 30.81606138205706458, -34.55876147768187678, 70.30501292735635843 ) ) ;
#23108 = CIRCLE ( 'NONE', #16944, 1.500000000000001332 ) ;
#23109 = ORIENTED_EDGE ( 'NONE', *, *, #17756, .F. ) ;
#23110 = ORIENTED_EDGE ( 'NONE', *, *, #1239, .F. ) ;
#23111 = LINE ( 'NONE', #5727, #18658 ) ;
#23112 = CARTESIAN_POINT ( 'NONE',  ( 36.31606138205702194, -19.34838015056931226, 26.94402965816085072 ) ) ;
#23113 = AXIS2_PLACEMENT_3D ( 'NONE', #18183, #6075, #10829 ) ;
#23114 = CARTESIAN_POINT ( 'NONE',  ( 38.82593461698264292, -26.70384086642191335, 73.13360434286902034 ) ) ;
#23115 = DIRECTION ( 'NONE',  ( -1.000000000000000000, 0.000000000000000000, 0.000000000000000000 ) ) ;
#23116 = ORIENTED_EDGE ( 'NONE', *, *, #18849, .T. ) ;
#23117 = CARTESIAN_POINT ( 'NONE',  ( 33.03722820848892638, 1.142818861812999742, 82.55501292736998664 ) ) ;
#23118 = FACE_OUTER_BOUND ( 'NONE', #21259, .T. ) ;
#23119 = CARTESIAN_POINT ( 'NONE',  ( 43.81606138205700063, 2.191238522347003226, 70.30501292737000085 ) ) ;
#23120 = EDGE_CURVE ( 'NONE', #23982, #16840, #7803, .T. ) ;
#23121 =( NAMED_UNIT ( * ) SI_UNIT ( $, .STERADIAN. ) SOLID_ANGLE_UNIT ( ) );
#23122 = ORIENTED_EDGE ( 'NONE', *, *, #24052, .T. ) ;
#23123 = CARTESIAN_POINT ( 'NONE',  ( 45.61606138205700489, 36.92314894770294131, 81.17823623207323180 ) ) ;
#23124 = VERTEX_POINT ( 'NONE', #3793 ) ;
#23125 = ORIENTED_EDGE ( 'NONE', *, *, #10543, .T. ) ;
#23126 = VECTOR ( 'NONE', #23667, 1000.000000000000000 ) ;
#23127 = LINE ( 'NONE', #11811, #24553 ) ;
#23128 = CARTESIAN_POINT ( 'NONE',  ( 37.25260217561390874, -9.613682088886102761, 71.78268878715394408 ) ) ;
#23129 = CARTESIAN_POINT ( 'NONE',  ( 38.00113996487114321, -11.91368208888610170, 72.53360434286904024 ) ) ;
#23130 = VERTEX_POINT ( 'NONE', #21080 ) ;
#23131 = VERTEX_POINT ( 'NONE', #9246 ) ;
#23132 = VECTOR ( 'NONE', #17992, 1000.000000000000000 ) ;
#23133 = DIRECTION ( 'NONE',  ( 0.000000000000000000, -2.999999999999999839E-15, -1.000000000000000000 ) ) ;
#23134 = DIRECTION ( 'NONE',  ( -1.786044098272412642E-16, -0.4425581086832399702, 0.8967398287344628960 ) ) ;
#23135 = CARTESIAN_POINT ( 'NONE',  ( 38.93415946300896024, -21.50384086642190340, 69.66206559358661821 ) ) ;
#23136 = LINE ( 'NONE', #11571, #17794 ) ;
#23137 = AXIS2_PLACEMENT_3D ( 'NONE', #1256, #16455, #20585 ) ;
#23138 = AXIS2_PLACEMENT_3D ( 'NONE', #16451, #14780, #18906 ) ;
#23139 = CARTESIAN_POINT ( 'NONE',  ( 39.41296390513587511, -16.41368208888610525, 71.67976084211551324 ) ) ;
#23140 = EDGE_LOOP ( 'NONE', ( #19971, #7557, #12853, #22611 ) ) ;
#23141 = LINE ( 'NONE', #21101, #22757 ) ;
#23142 = EDGE_CURVE ( 'NONE', #17733, #559, #10117, .T. ) ;
#23143 = CARTESIAN_POINT ( 'NONE',  ( 38.31606138205694378, 2.926944320371558383, 0.2449088955976189141 ) ) ;
#23144 = VECTOR ( 'NONE', #16822, 1000.000000000000000 ) ;
#23145 = DIRECTION ( 'NONE',  ( -1.000000000000000000, -3.091505625455828697E-15, -4.515976121274772923E-17 ) ) ;
#23146 = CARTESIAN_POINT ( 'NONE',  ( 39.54057891361352972, -5.597689502044176812, 82.79751455073319732 ) ) ;
#23147 = DIRECTION ( 'NONE',  ( -1.445602896647339656E-16, 0.8212051873014208914, 0.5706330172266919076 ) ) ;
#23148 = VECTOR ( 'NONE', #18997, 1000.000000000000000 ) ;
#23149 = DIRECTION ( 'NONE',  ( 0.000000000000000000, -0.5706330172266907974, 0.8212051873014217795 ) ) ;
#23150 = EDGE_LOOP ( 'NONE', ( #7082, #24476 ) ) ;
#23151 = DIRECTION ( 'NONE',  ( -1.000000000000000000, 1.115179377413661005E-30, 3.717264591378870232E-16 ) ) ;
#23152 = AXIS2_PLACEMENT_3D ( 'NONE', #16297, #12208, #20052 ) ;
#23153 = CARTESIAN_POINT ( 'NONE',  ( 45.81606138205707879, -39.99575152356564445, 63.13209164280871022 ) ) ;
#23154 = VERTEX_POINT ( 'NONE', #17975 ) ;
#23155 = ORIENTED_EDGE ( 'NONE', *, *, #141, .T. ) ;
#23156 = CARTESIAN_POINT ( 'NONE',  ( 40.33642880535521869, -13.30384086642190944, 69.98269868914866265 ) ) ;
#23157 = DIRECTION ( 'NONE',  ( 1.000000000000000275E-15, -0.9439899321577401858, -0.3299742535180970604 ) ) ;
#23158 = CARTESIAN_POINT ( 'NONE',  ( 39.95015449827720744, -12.61368208888610454, 70.79240656858105751 ) ) ;
#23159 = VECTOR ( 'NONE', #2075, 1000.000000000000000 ) ;
#23160 = VERTEX_POINT ( 'NONE', #21958 ) ;
#23161 = LINE ( 'NONE', #5650, #8880 ) ;
#23162 = LINE ( 'NONE', #3583, #2622 ) ;
#23163 = VECTOR ( 'NONE', #15217, 1000.000000000000000 ) ;
#23164 = CARTESIAN_POINT ( 'NONE',  ( 39.12911128074873801, -22.11368208888610809, 73.69843995877327814 ) ) ;
#23165 = ORIENTED_EDGE ( 'NONE', *, *, #22490, .T. ) ;
#23166 = EDGE_CURVE ( 'NONE', #15622, #3232, #8310, .T. ) ;
#23167 = LINE ( 'NONE', #9410, #3221 ) ;
#23168 = EDGE_CURVE ( 'NONE', #19007, #5938, #19771, .T. ) ;
#23169 = LINE ( 'NONE', #24959, #22598 ) ;
#23170 = CARTESIAN_POINT ( 'NONE',  ( 33.33121445922205339, -32.87633672316712108, 59.29685926994373091 ) ) ;
#23171 = VECTOR ( 'NONE', #6860, 1000.000000000000000 ) ;
#23172 = ADVANCED_FACE ( 'NONE', ( #2362 ), #21702, .T. ) ;
#23173 = MECHANICAL_DESIGN_GEOMETRIC_PRESENTATION_REPRESENTATION (  '', ( #5508 ), #4671 ) ;
#23174 = DIRECTION ( 'NONE',  ( -1.836970198721029688E-16, -2.999999999999999839E-15, -1.000000000000000000 ) ) ;
#23175 = VECTOR ( 'NONE', #21379, 1000.000000000000000 ) ;
#23176 = CARTESIAN_POINT ( 'NONE',  ( 45.81606138205706458, -34.54722833698617990, 70.28164373264664277 ) ) ;
#23177 = CARTESIAN_POINT ( 'NONE',  ( 37.38336156205273397, -11.90384086642191441, 70.63227792289247020 ) ) ;
#23178 = CARTESIAN_POINT ( 'NONE',  ( 40.14115730948191185, -2.513682088886103116, 71.32335560751961623 ) ) ;
#23179 = VERTEX_POINT ( 'NONE', #16025 ) ;
#23180 = DIRECTION ( 'NONE',  ( -1.000000000000000000, 0.000000000000000000, 0.000000000000000000 ) ) ;
#23181 = EDGE_CURVE ( 'NONE', #4360, #25460, #19328, .T. ) ;
#23182 = VECTOR ( 'NONE', #23040, 1000.000000000000000 ) ;
#23183 = DIRECTION ( 'NONE',  ( 1.445602896647339903E-16, -1.000000000000000000, 2.999999999999999839E-15 ) ) ;
#23184 = ORIENTED_EDGE ( 'NONE', *, *, #8727, .F. ) ;
#23185 = ORIENTED_EDGE ( 'NONE', *, *, #6762, .F. ) ;
#23186 = CARTESIAN_POINT ( 'NONE',  ( 39.38009889167648936, -1.403840866421906419, 70.00779233799264034 ) ) ;
#23187 = CARTESIAN_POINT ( 'NONE',  ( 38.82593461698262871, 1.086317911113899637, 69.62690120949091011 ) ) ;
#23188 = CARTESIAN_POINT ( 'NONE',  ( 39.64521430340304420, -2.813682088886101162, 69.45876917294177133 ) ) ;
#23189 = ORIENTED_EDGE ( 'NONE', *, *, #15709, .T. ) ;
#23190 = CARTESIAN_POINT ( 'NONE',  ( 31.81606138205700418, 40.39281886181299797, 81.75501292736983316 ) ) ;
#23191 = CARTESIAN_POINT ( 'NONE',  ( 39.51027997493896748, -3.103840866421909706, 71.43714994484034264 ) ) ;
#23192 = CARTESIAN_POINT ( 'NONE',  ( 33.81606138205700063, 15.19123852234701388, 73.80501292736995822 ) ) ;
#23193 = ORIENTED_EDGE ( 'NONE', *, *, #4215, .F. ) ;
#23194 = DIRECTION ( 'NONE',  ( 3.469446951953614189E-15, -0.8967398287344635621, -0.4425581086832386379 ) ) ;
#23195 = DIRECTION ( 'NONE',  ( 0.000000000000000000, 1.000000000000000000, -6.938893903907222067E-15 ) ) ;
#23196 = CARTESIAN_POINT ( 'NONE',  ( 37.50301148336529877, -10.50384086642191761, 73.69843995877330656 ) ) ;
#23197 = AXIS2_PLACEMENT_3D ( 'NONE', #14734, #20669, #17068 ) ;
#23198 = CARTESIAN_POINT ( 'NONE',  ( 44.06606138205700063, -26.74044063519535186, 82.55501292737007191 ) ) ;
#23199 = CARTESIAN_POINT ( 'NONE',  ( 38.31606138205700773, -21.82678658219787948, 29.70634659473178019 ) ) ;
#23200 = CARTESIAN_POINT ( 'NONE',  ( 37.33957961208646736, -13.81368208888610916, 72.81632618279321889 ) ) ;
#23201 = CARTESIAN_POINT ( 'NONE',  ( 43.81606138205700063, -35.70002751211045933, 71.94742330197156832 ) ) ;
#23202 = VECTOR ( 'NONE', #21437, 1000.000000000000000 ) ;
#23203 = CARTESIAN_POINT ( 'NONE',  ( 29.81606138205707168, -37.26069504592558701, 64.48189387429259511 ) ) ;
#23204 = ORIENTED_EDGE ( 'NONE', *, *, #5793, .T. ) ;
#23205 = CARTESIAN_POINT ( 'NONE',  ( 30.81606138205705037, -30.46100403034035509, 72.05704881431053366 ) ) ;
#23206 = CARTESIAN_POINT ( 'NONE',  ( 38.37017380507018771, -7.603840866421906597, 69.64448340153879258 ) ) ;
#23207 = APPLICATION_PROTOCOL_DEFINITION ( 'draft international standard', 'automotive_design', 1998, #3876 ) ;
#23208 = DIRECTION ( 'NONE',  ( -1.734723475976804876E-16, -3.491481338843135327E-15, -1.000000000000000000 ) ) ;
#23209 = CARTESIAN_POINT ( 'NONE',  ( 37.80618814713140097, -15.91368208888610880, 73.13360434286903455 ) ) ;
#23210 = PRODUCT_DEFINITION_FORMATION_WITH_SPECIFIED_SOURCE ( 'ANY', '', #19375, .NOT_KNOWN. ) ;
#23211 = CARTESIAN_POINT ( 'NONE',  ( 40.31606138205700773, -10.19550266980813014, 14.63954348514304904 ) ) ;
#23212 = EDGE_CURVE ( 'NONE', #4421, #16465, #10239, .T. ) ;
#23213 = CIRCLE ( 'NONE', #12143, 1.000000000000000888 ) ;
#23214 = CARTESIAN_POINT ( 'NONE',  ( 36.49096545463212493, -20.10384086642191193, 71.32335560751961623 ) ) ;
#23215 = PLANE ( 'NONE',  #21269 ) ;
#23216 = CARTESIAN_POINT ( 'NONE',  ( 39.95015449827720744, -20.61368208888610454, 70.79240656858105751 ) ) ;
#23217 = ORIENTED_EDGE ( 'NONE', *, *, #13806, .F. ) ;
#23218 = CARTESIAN_POINT ( 'NONE',  ( 38.26194895904383486, -25.01368208888610312, 69.04448340153878405 ) ) ;
#23219 = ORIENTED_EDGE ( 'NONE', *, *, #4337, .F. ) ;
#23220 = CARTESIAN_POINT ( 'NONE',  ( 45.06606138205697221, -5.022037326221688858, -5.474317061061731771 ) ) ;
#23221 = VECTOR ( 'NONE', #18909, 1000.000000000000000 ) ;
#23222 = CARTESIAN_POINT ( 'NONE',  ( 31.81606138205700418, 39.39281886181299797, 81.75501292736984738 ) ) ;
#23223 = CARTESIAN_POINT ( 'NONE',  ( 39.02742774030101458, -27.40384086642191619, 70.49320253461758057 ) ) ;
#23224 = ORIENTED_EDGE ( 'NONE', *, *, #9177, .F. ) ;
#23225 = ORIENTED_EDGE ( 'NONE', *, *, #23733, .T. ) ;
#23226 = DIRECTION ( 'NONE',  ( 0.000000000000000000, -0.1918498038142812112, 0.9814242980364923374 ) ) ;
#23227 = CARTESIAN_POINT ( 'NONE',  ( 43.23147868389327897, 41.90149715599300606, 79.37823623207322044 ) ) ;
#23228 = VERTEX_POINT ( 'NONE', #6244 ) ;
#23229 = DIRECTION ( 'NONE',  ( -9.027796614315171564E-31, -1.000000000000000000, -1.163336342344335610E-15 ) ) ;
#23230 = CARTESIAN_POINT ( 'NONE',  ( 39.98359781491296161, -1.203840866421911127, 70.89533451361947414 ) ) ;
#23231 = ADVANCED_FACE ( 'NONE', ( #23498 ), #4441, .F. ) ;
#23232 = DIRECTION ( 'NONE',  ( 9.027796614315171564E-31, 1.000000000000000000, 4.694469519536151390E-16 ) ) ;
#23233 = ADVANCED_FACE ( 'NONE', ( #14104 ), #4322, .F. ) ;
#23234 = CYLINDRICAL_SURFACE ( 'NONE', #8143, 1.750000000000001554 ) ;
#23235 = EDGE_LOOP ( 'NONE', ( #12487, #1066, #7827, #16552 ) ) ;
#23236 = AXIS2_PLACEMENT_3D ( 'NONE', #21791, #19597, #17295 ) ;
#23237 = EDGE_CURVE ( 'NONE', #13134, #25120, #6584, .T. ) ;
#23238 = ORIENTED_EDGE ( 'NONE', *, *, #4139, .T. ) ;
#23239 = CYLINDRICAL_SURFACE ( 'NONE', #10446, 3.000000000000002665 ) ;
#23240 = CARTESIAN_POINT ( 'NONE',  ( 43.31606138205700063, -37.98241563432385703, 69.85268917996594951 ) ) ;
#23241 = CARTESIAN_POINT ( 'NONE',  ( 39.98359781491296161, -27.20384086642191335, 70.89533451361944572 ) ) ;
#23242 = SURFACE_SIDE_STYLE ('',( #15137 ) ) ;
#23243 = DIRECTION ( 'NONE',  ( 0.000000000000000000, -1.000000000000000000, 3.491481338843135327E-15 ) ) ;
#23244 = ORIENTED_EDGE ( 'NONE', *, *, #8071, .F. ) ;
#23245 = CARTESIAN_POINT ( 'NONE',  ( 40.56606138205700773, 5.308699250829721272, 2.416607620847027960 ) ) ;
#23246 = EDGE_CURVE ( 'NONE', #13742, #545, #5867, .T. ) ;
#23247 = FACE_OUTER_BOUND ( 'NONE', #18922, .T. ) ;
#23248 = DIRECTION ( 'NONE',  ( -2.168404344971010101E-16, 0.8212051873014210024, 0.5706330172266920187 ) ) ;
#23249 = CARTESIAN_POINT ( 'NONE',  ( 37.38336156205273397, -7.903840866421910860, 70.63227792289248441 ) ) ;
#23250 = ORIENTED_EDGE ( 'NONE', *, *, #5796, .T. ) ;
#23251 = LINE ( 'NONE', #15275, #17744 ) ;
#23252 = EDGE_LOOP ( 'NONE', ( #21741, #13069, #5842, #5396 ) ) ;
#23253 = ORIENTED_EDGE ( 'NONE', *, *, #10334, .T. ) ;
#23254 = AXIS2_PLACEMENT_3D ( 'NONE', #7336, #11466, #9783 ) ;
#23255 = DIRECTION ( 'NONE',  ( -1.000000000000000000, -2.999999999999999839E-15, 0.000000000000000000 ) ) ;
#23256 = CARTESIAN_POINT ( 'NONE',  ( 38.26194895904383486, -15.01368208888610134, 70.24448340153875847 ) ) ;
#23257 = CARTESIAN_POINT ( 'NONE',  ( 37.38336156205274818, -9.713682088886098853, 72.12822762946751709 ) ) ;
#23258 = EDGE_LOOP ( 'NONE', ( #4099, #18002, #4640, #18498 ) ) ;
#23259 = ORIENTED_EDGE ( 'NONE', *, *, #23552, .F. ) ;
#23260 = CARTESIAN_POINT ( 'NONE',  ( 31.81606138205700418, -34.55876147765400930, 73.55501292737011454 ) ) ;
#23261 = CARTESIAN_POINT ( 'NONE',  ( 39.31606138205697931, -10.17000407126883843, 36.59108960988216808 ) ) ;
#23262 = ORIENTED_EDGE ( 'NONE', *, *, #20629, .T. ) ;
#23263 = CARTESIAN_POINT ( 'NONE',  ( 39.29254315202756231, 1.186317911113898838, 69.94417936956675419 ) ) ;
#23264 = CARTESIAN_POINT ( 'NONE',  ( 40.14115730948191185, -17.10384086642191193, 71.43714994484030001 ) ) ;
#23265 = EDGE_CURVE ( 'NONE', #1793, #16154, #4188, .T. ) ;
#23266 = EDGE_CURVE ( 'NONE', #18450, #13333, #20153, .T. ) ;
#23267 = CARTESIAN_POINT ( 'NONE',  ( 33.31606138205698642, -7.467730535347551601, -2.778285769174305919 ) ) ;
#23268 = CARTESIAN_POINT ( 'NONE',  ( 37.31647492878122563, -21.31368208888610027, 70.72433947564853440 ) ) ;
#23269 = EDGE_CURVE ( 'NONE', #25152, #1727, #24000, .T. ) ;
#23270 = EDGE_CURVE ( 'NONE', #16929, #13742, #8057, .T. ) ;
#23271 = EDGE_CURVE ( 'NONE', #14131, #21718, #14406, .T. ) ;
#23272 = EDGE_LOOP ( 'NONE', ( #4065, #1919, #23417, #14545 ) ) ;
#23273 = DIRECTION ( 'NONE',  ( 1.000000000000000000, 2.602085213965208275E-15, 0.000000000000000000 ) ) ;
#23274 = CARTESIAN_POINT ( 'NONE',  ( 36.06606138205700063, 5.594015759443068170, 2.006005027196319901 ) ) ;
#23275 = CARTESIAN_POINT ( 'NONE',  ( 32.81606138205700773, -34.55876147765401640, 70.30501292737011454 ) ) ;
#23276 = CARTESIAN_POINT ( 'NONE',  ( 40.31606138205700773, -7.204193249396275256, 83.11277699141410835 ) ) ;
#23277 = DIRECTION ( 'NONE',  ( 0.000000000000000000, 0.7540134720837716742, 0.6568589528324746407 ) ) ;
#23278 = ADVANCED_FACE ( 'NONE', ( #10363 ), #18228, .F. ) ;
#23279 = CARTESIAN_POINT ( 'NONE',  ( 45.81606138205697221, -4.589472609077215992, -6.350807634294792337 ) ) ;
#23280 =( REPRESENTATION_RELATIONSHIP ('NONE','NONE', #17377, #18165 ) REPRESENTATION_RELATIONSHIP_WITH_TRANSFORMATION ( #8271 )SHAPE_REPRESENTATION_RELATIONSHIP( ) );
#23281 = ORIENTED_EDGE ( 'NONE', *, *, #9395, .F. ) ;
#23282 = CARTESIAN_POINT ( 'NONE',  ( 40.31606138205700773, -7.108955154158179468, 82.62193108360246185 ) ) ;
#23283 = EDGE_LOOP ( 'NONE', ( #17605, #12161, #21954, #14593 ) ) ;
#23284 = ORIENTED_EDGE ( 'NONE', *, *, #17611, .T. ) ;
#23285 = CARTESIAN_POINT ( 'NONE',  ( 39.73277004305197124, -9.403840866421907307, 69.52238214136768590 ) ) ;
#23286 = DIRECTION ( 'NONE',  ( 0.000000000000000000, -1.000000000000000000, 3.491481338843135327E-15 ) ) ;
#23287 = CARTESIAN_POINT ( 'NONE',  ( 39.82603832034400426, -14.31368208888610916, 72.40698646996133903 ) ) ;
#23288 = ORIENTED_EDGE ( 'NONE', *, *, #21996, .T. ) ;
#23289 = DIRECTION ( 'NONE',  ( 0.000000000000000000, 1.000000000000000000, -2.999999999999999839E-15 ) ) ;
#23290 = CARTESIAN_POINT ( 'NONE',  ( 43.81606138205700063, 28.12806996228107081, 65.30501292736992980 ) ) ;
#23291 = CARTESIAN_POINT ( 'NONE',  ( 40.77203464402485622, -20.51368208888610667, 71.32335560751960202 ) ) ;
#23292 = DIRECTION ( 'NONE',  ( -1.445602896647339656E-16, 0.8212051873014208914, 0.5706330172266919076 ) ) ;
#23293 = CARTESIAN_POINT ( 'NONE',  ( 40.31606138205700773, 37.94123852234599781, 75.30501292736988717 ) ) ;
#23294 =( LENGTH_UNIT ( ) NAMED_UNIT ( * ) SI_UNIT ( .MILLI., .METRE. ) );
#23295 = DIRECTION ( 'NONE',  ( 1.000000000000000000, 2.999999999999999839E-15, 0.000000000000000000 ) ) ;
#23296 = DIRECTION ( 'NONE',  ( 1.000000000000000000, 2.999999999999999839E-15, 0.000000000000000000 ) ) ;
#23297 = CARTESIAN_POINT ( 'NONE',  ( 39.31564783533279694, -11.30384086642191299, 70.72433947564853440 ) ) ;
#23298 = CARTESIAN_POINT ( 'NONE',  ( 39.37952058850012804, -28.61368208888610454, 70.97781676520600058 ) ) ;
#23299 = ORIENTED_EDGE ( 'NONE', *, *, #8155, .T. ) ;
#23300 = CARTESIAN_POINT ( 'NONE',  ( 30.81606138205700418, -31.45856502260510013, 77.07494475056050476 ) ) ;
#23301 = CARTESIAN_POINT ( 'NONE',  ( 43.81606138205700063, -39.60075215179220720, 69.23691647014479145 ) ) ;
#23302 = EDGE_LOOP ( 'NONE', ( #23509, #8082, #5374, #16946 ) ) ;
#23303 = ORIENTED_EDGE ( 'NONE', *, *, #17984, .F. ) ;
#23304 = ADVANCED_FACE ( 'NONE', ( #13726 ), #13875, .T. ) ;
#23305 = CARTESIAN_POINT ( 'NONE',  ( 40.33642880535521869, -27.30384086642191477, 69.98269868914864844 ) ) ;
#23306 = ADVANCED_FACE ( 'NONE', ( #4694, #24375 ), #22587, .T. ) ;
#23307 = PRODUCT_DEFINITION ( 'UNKNOWN', '', #19938, #12130 ) ;
#23308 = CARTESIAN_POINT ( 'NONE',  ( 38.93415946300897446, -0.1136820888861071466, 73.09843995877331224 ) ) ;
#23309 = CARTESIAN_POINT ( 'NONE',  ( 35.86008812008917346, -1.513682088886105781, 71.43714994484035685 ) ) ;
#23310 = EDGE_LOOP ( 'NONE', ( #17035, #9843, #13642, #14689, #15340, #4446 ) ) ;
#23311 = CARTESIAN_POINT ( 'NONE',  ( 40.56606138205696510, -1.522470315718718270, 0.9921758631592225708 ) ) ;
#23312 = AXIS2_PLACEMENT_3D ( 'NONE', #16294, #18251, #18000 ) ;
#23313 = CARTESIAN_POINT ( 'NONE',  ( 39.51027997493896748, -7.103840866421911038, 71.43714994484034264 ) ) ;
#23314 = AXIS2_PLACEMENT_3D ( 'NONE', #2103, #17845, #173 ) ;
#23315 = VECTOR ( 'NONE', #14236, 1000.000000000000000 ) ;
#23316 = FACE_OUTER_BOUND ( 'NONE', #25066, .T. ) ;
#23317 = VERTEX_POINT ( 'NONE', #22336 ) ;
#23318 = LINE ( 'NONE', #9439, #197 ) ;
#23319 = CARTESIAN_POINT ( 'NONE',  ( 37.31606138205700063, 43.19123852234595518, 61.30501292736988006 ) ) ;
#23320 = CARTESIAN_POINT ( 'NONE',  ( 35.86008812008917346, -10.10384086642191548, 71.32335560751961623 ) ) ;
#23321 = CYLINDRICAL_SURFACE ( 'NONE', #16437, 1.500000000000001332 ) ;
#23322 = CARTESIAN_POINT ( 'NONE',  ( 37.80618814713140097, -11.91368208888611058, 73.13360434286903455 ) ) ;
#23323 = CYLINDRICAL_SURFACE ( 'NONE', #17504, 1.000000000000000888 ) ;
#23324 = EDGE_CURVE ( 'NONE', #20889, #64, #14479, .T. ) ;
#23325 = DIRECTION ( 'NONE',  ( 0.000000000000000000, -0.7540134720837718962, -0.6568589528324743076 ) ) ;
#23326 = VERTEX_POINT ( 'NONE', #10623 ) ;
#23327 = DIRECTION ( 'NONE',  ( 0.000000000000000000, -1.000000000000000000, 2.999999999999999839E-15 ) ) ;
#23328 = CARTESIAN_POINT ( 'NONE',  ( 39.82603832034401137, -1.303840866421906775, 70.35351908239860563 ) ) ;
#23329 = AXIS2_PLACEMENT_3D ( 'NONE', #25243, #13420, #15593 ) ;
#23330 = APPLICATION_PROTOCOL_DEFINITION ( 'draft international standard', 'automotive_design', 1998, #6515 ) ;
#23331 = CARTESIAN_POINT ( 'NONE',  ( 33.31606138205700773, 3.996716213179724697, 6.311483552851885115 ) ) ;
#23332 = CARTESIAN_POINT ( 'NONE',  ( 38.37017380507020192, -20.01368208888610667, 73.11602215082116629 ) ) ;
#23333 = AXIS2_PLACEMENT_3D ( 'NONE', #12682, #801, #16918 ) ;
#23334 = CIRCLE ( 'NONE', #4829, 10.50000000000000000 ) ;
#23335 = CARTESIAN_POINT ( 'NONE',  ( 34.06606138205700773, -36.11063010576116739, 71.66210679335823386 ) ) ;
#23336 = EDGE_CURVE ( 'NONE', #7351, #643, #18474, .T. ) ;
#23337 = CARTESIAN_POINT ( 'NONE',  ( 36.80608444377001831, -18.30384086642190766, 72.40698646996135324 ) ) ;
#23338 = LINE ( 'NONE', #19229, #14283 ) ;
#23339 = EDGE_CURVE ( 'NONE', #2531, #24390, #11229, .T. ) ;
#23340 = CARTESIAN_POINT ( 'NONE',  ( 38.26194895904383486, -19.01368208888610312, 69.64448340153877837 ) ) ;
#23341 = ORIENTED_EDGE ( 'NONE', *, *, #19314, .F. ) ;
#23342 = CARTESIAN_POINT ( 'NONE',  ( 39.73277004305198545, -20.21368208888611306, 73.23812341099225875 ) ) ;
#23343 = ORIENTED_EDGE ( 'NONE', *, *, #251, .F. ) ;
#23344 = CARTESIAN_POINT ( 'NONE',  ( 38.31606138205700063, -11.51539968388051882, 18.41550321377400934 ) ) ;
#23345 = DIRECTION ( 'NONE',  ( -9.027796614315171564E-31, -1.000000000000000000, -3.938893903907230117E-15 ) ) ;
#23346 = CARTESIAN_POINT ( 'NONE',  ( 38.37017380507018771, -21.60384086642191548, 70.24448340153875847 ) ) ;
#23347 = VERTEX_POINT ( 'NONE', #16527 ) ;
#23348 = ORIENTED_EDGE ( 'NONE', *, *, #19495, .F. ) ;
#23349 = CARTESIAN_POINT ( 'NONE',  ( 39.81746892067405952, 40.76768529863396395, 79.57823623207323749 ) ) ;
#23350 = DIRECTION ( 'NONE',  ( 1.000000000000000000, 8.911169920151748851E-16, 3.114923731923493702E-16 ) ) ;
#23351 = DIRECTION ( 'NONE',  ( -1.000000000000000000, -3.243061817617045614E-15, -1.199556157213611407E-16 ) ) ;
#23352 = CARTESIAN_POINT ( 'NONE',  ( 40.52078840805429394, -29.00384086642191406, 72.15350918040381600 ) ) ;
#23353 = AXIS2_PLACEMENT_3D ( 'NONE', #16062, #16435, #21870 ) ;
#23354 = VECTOR ( 'NONE', #1312, 1000.000000000000000 ) ;
#23355 = DIRECTION ( 'NONE',  ( -2.048868001712896742E-15, 0.6595716529892345914, -0.7516416929448823669 ) ) ;
#23356 = CARTESIAN_POINT ( 'NONE',  ( 39.12911128074873801, -4.113682088886107202, 73.69843995877330656 ) ) ;
#23357 = EDGE_CURVE ( 'NONE', #12767, #17582, #16274, .T. ) ;
#23358 = CARTESIAN_POINT ( 'NONE',  ( 30.81606138205698642, -6.548589660139424673, -8.069948661059610728 ) ) ;
#23359 = ORIENTED_EDGE ( 'NONE', *, *, #13519, .F. ) ;
#23360 = VERTEX_POINT ( 'NONE', #23055 ) ;
#23361 = DIRECTION ( 'NONE',  ( -1.734723475976804876E-16, -3.491481338843135327E-15, -1.000000000000000000 ) ) ;
#23362 = CARTESIAN_POINT ( 'NONE',  ( 41.06606138205703616, -24.72749677399387735, 32.19456755146972426 ) ) ;
#23363 = ORIENTED_EDGE ( 'NONE', *, *, #19791, .T. ) ;
#23364 = CARTESIAN_POINT ( 'NONE',  ( 38.37017380507018771, -25.60384086642190837, 69.64448340153876416 ) ) ;
#23365 =( NAMED_UNIT ( * ) PLANE_ANGLE_UNIT ( ) SI_UNIT ( $, .RADIAN. ) );
#23366 = DIRECTION ( 'NONE',  ( 0.000000000000000000, -0.5735764363510444941, 0.8191520442889929088 ) ) ;
#23367 = EDGE_LOOP ( 'NONE', ( #162, #8769, #15374, #9902 ) ) ;
#23368 = CARTESIAN_POINT ( 'NONE',  ( 38.44255644662678861, -39.60718113818700203, 83.30501292737011454 ) ) ;
#23369 = CARTESIAN_POINT ( 'NONE',  ( 43.31097620601923381, -33.12114953149411178, 59.73560708446377987 ) ) ;
#23370 = CARTESIAN_POINT ( 'NONE',  ( 33.31606138205700773, 10.06218483883314718, 67.80501292737497465 ) ) ;
#23371 = CARTESIAN_POINT ( 'NONE',  ( 39.51027997493896748, -5.103840866421911926, 71.43714994484034264 ) ) ;
#23372 = ORIENTED_EDGE ( 'NONE', *, *, #16483, .F. ) ;
#23373 = VECTOR ( 'NONE', #3564, 1000.000000000000227 ) ;
#23374 = DIRECTION ( 'NONE',  ( -1.000000000000000000, -2.699773532888683051E-15, -2.369073068322443402E-15 ) ) ;
#23375 = ORIENTED_EDGE ( 'NONE', *, *, #12217, .T. ) ;
#23376 = ORIENTED_EDGE ( 'NONE', *, *, #15511, .F. ) ;
#23377 = LINE ( 'NONE', #3801, #25386 ) ;
#23378 = CARTESIAN_POINT ( 'NONE',  ( 38.63098279924288647, -12.91368208888610525, 70.22690120949090442 ) ) ;
#23379 = CARTESIAN_POINT ( 'NONE',  ( 38.26194895904383486, -9.013682088886101340, 70.24448340153877268 ) ) ;
#23380 = ORIENTED_EDGE ( 'NONE', *, *, #16339, .F. ) ;
#23381 = ORIENTED_EDGE ( 'NONE', *, *, #20044, .T. ) ;
#23382 = CYLINDRICAL_SURFACE ( 'NONE', #19792, 10.00000000000000000 ) ;
#23383 = DIRECTION ( 'NONE',  ( 1.000000000000000000, 0.000000000000000000, 0.000000000000000000 ) ) ;
#23384 = CYLINDRICAL_SURFACE ( 'NONE', #1285, 1.500000000000000222 ) ;
#23385 = CARTESIAN_POINT ( 'NONE',  ( 39.82603832034400426, -17.30384086642190056, 70.35351908239857721 ) ) ;
#23386 =( GEOMETRIC_REPRESENTATION_CONTEXT ( 3 ) GLOBAL_UNCERTAINTY_ASSIGNED_CONTEXT ( ( #6129 ) ) GLOBAL_UNIT_ASSIGNED_CONTEXT ( ( #12706, #22226, #6769 ) ) REPRESENTATION_CONTEXT ( 'NONE', 'WORKASPACE' ) );
#23387 = CARTESIAN_POINT ( 'NONE',  ( 41.31606138205700063, 14.21032488318011211, 61.14033482768515881 ) ) ;
#23388 = EDGE_CURVE ( 'NONE', #3808, #1739, #3481, .T. ) ;
#23389 = CARTESIAN_POINT ( 'NONE',  ( 38.26194895904383486, -21.01368208888610312, 70.24448340153875847 ) ) ;
#23390 = ORIENTED_EDGE ( 'NONE', *, *, #16028, .F. ) ;
#23391 = CIRCLE ( 'NONE', #16403, 1.000000000000000888 ) ;
#23392 = DIRECTION ( 'NONE',  ( 1.000000000000000000, 0.000000000000000000, 0.000000000000000000 ) ) ;
#23393 = CARTESIAN_POINT ( 'NONE',  ( 36.68196826583682935, -11.61368208888610276, 71.96809898377888715 ) ) ;
#23394 = DIRECTION ( 'NONE',  ( 0.000000000000000000, -1.000000000000000000, 0.000000000000000000 ) ) ;
#23395 = DIRECTION ( 'NONE',  ( -2.048868001712896742E-15, 0.6595716529892345914, -0.7516416929448823669 ) ) ;
#23396 = AXIS2_PLACEMENT_3D ( 'NONE', #7471, #19572, #23048 ) ;
#23397 = CARTESIAN_POINT ( 'NONE',  ( 38.57734783014581836, -5.216956884619976087, 83.31008680947429923 ) ) ;
#23398 = FACE_OUTER_BOUND ( 'NONE', #18995, .T. ) ;
#23399 = VECTOR ( 'NONE', #13031, 1000.000000000000000 ) ;
#23400 = DIRECTION ( 'NONE',  ( 0.000000000000000000, 1.000000000000000000, 0.000000000000000000 ) ) ;
#23401 = EDGE_CURVE ( 'NONE', #19565, #9905, #19080, .T. ) ;
#23402 = ORIENTED_EDGE ( 'NONE', *, *, #9873, .F. ) ;
#23403 = EDGE_CURVE ( 'NONE', #18110, #16336, #22459, .T. ) ;
#23404 = LINE ( 'NONE', #1762, #12380 ) ;
#23405 = EDGE_LOOP ( 'NONE', ( #13459, #14267, #24943, #25410 ) ) ;
#23406 = EDGE_CURVE ( 'NONE', #22767, #19154, #6495, .T. ) ;
#23407 = ORIENTED_EDGE ( 'NONE', *, *, #8159, .F. ) ;
#23408 = CARTESIAN_POINT ( 'NONE',  ( 37.50301148336529877, -12.50384086642191939, 73.69843995877327814 ) ) ;
#23409 = EDGE_CURVE ( 'NONE', #17216, #16296, #11357, .T. ) ;
#23410 = EDGE_CURVE ( 'NONE', #3683, #21091, #20402, .T. ) ;
#23411 = AXIS2_PLACEMENT_3D ( 'NONE', #24465, #14323, #12276 ) ;
#23412 = ORIENTED_EDGE ( 'NONE', *, *, #4695, .F. ) ;
#23413 = CARTESIAN_POINT ( 'NONE',  ( 37.31606138205700063, 43.19123852234596939, 66.30501292736988717 ) ) ;
#23414 = CARTESIAN_POINT ( 'NONE',  ( 36.87297107704152666, -11.71368208888611129, 72.49904802271740323 ) ) ;
#23415 = TOROIDAL_SURFACE ( 'NONE', #16008, 0.9023161253044896801, 0.2000000000000000111 ) ;
#23416 =( NAMED_UNIT ( * ) SI_UNIT ( $, .STERADIAN. ) SOLID_ANGLE_UNIT ( ) );
#23417 = ORIENTED_EDGE ( 'NONE', *, *, #5849, .F. ) ;
#23418 = LINE ( 'NONE', #13397, #2978 ) ;
#23419 = PLANE ( 'NONE',  #3462 ) ;
#23420 = ADVANCED_FACE ( 'NONE', ( #24247 ), #807, .T. ) ;
#23421 = CARTESIAN_POINT ( 'NONE',  ( 39.64521430340304420, -20.81368208888610027, 69.45876917294175712 ) ) ;
#23422 = EDGE_CURVE ( 'NONE', #19611, #13467, #12689, .T. ) ;
#23423 = ORIENTED_EDGE ( 'NONE', *, *, #839, .T. ) ;
#23424 = AXIS2_PLACEMENT_3D ( 'NONE', #14014, #14142, #15813 ) ;
#23425 = LINE ( 'NONE', #6044, #18874 ) ;
#23426 = AXIS2_PLACEMENT_3D ( 'NONE', #14407, #4117, #12495 ) ;
#23427 = LINE ( 'NONE', #21502, #16848 ) ;
#23428 = LINE ( 'NONE', #11734, #7517 ) ;
#23429 = DIRECTION ( 'NONE',  ( 0.000000000000000000, -0.1918498038142821827, 0.9814242980364921154 ) ) ;
#23430 = VECTOR ( 'NONE', #2244, 1000.000000000000114 ) ;
#23431 = DIRECTION ( 'NONE',  ( -0.000000000000000000, 0.5735764363510447161, -0.8191520442889929088 ) ) ;
#23432 = EDGE_CURVE ( 'NONE', #21114, #2595, #18116, .T. ) ;
#23433 = CARTESIAN_POINT ( 'NONE',  ( 43.06277394478077269, 3.412914273465426973, 6.350629194390777776 ) ) ;
#23434 = VECTOR ( 'NONE', #4817, 1000.000000000000000 ) ;
#23435 = CARTESIAN_POINT ( 'NONE',  ( 37.60469502381300799, -12.40384086642191441, 72.26730301774234988 ) ) ;
#23436 = CARTESIAN_POINT ( 'NONE',  ( 38.37017380507020192, -2.013682088886109334, 73.11602215082118050 ) ) ;
#23437 = ORIENTED_EDGE ( 'NONE', *, *, #10660, .F. ) ;
#23438 = CARTESIAN_POINT ( 'NONE',  ( 40.11656585159207822, -21.15827616857647797, 75.86899733230406184 ) ) ;
#23439 = CARTESIAN_POINT ( 'NONE',  ( 43.31606138205700063, -35.82531359714782582, 71.25150419970752580 ) ) ;
#23440 = ORIENTED_EDGE ( 'NONE', *, *, #24334, .T. ) ;
#23441 = EDGE_LOOP ( 'NONE', ( #18078, #7066, #9661, #8474, #5999 ) ) ;
#23442 = AXIS2_PLACEMENT_3D ( 'NONE', #14293, #24185, #362 ) ;
#23443 = CARTESIAN_POINT ( 'NONE',  ( 38.26194895904384907, 1.396159133578083633, 73.11602215082119471 ) ) ;
#23444 = CARTESIAN_POINT ( 'NONE',  ( 37.69225076346193504, -25.81368208888610027, 72.33091598616823603 ) ) ;
#23445 = CARTESIAN_POINT ( 'NONE',  ( 39.02088643472237095, -4.913682088886102584, 69.02690120949094421 ) ) ;
#23446 = AXIS2_PLACEMENT_3D ( 'NONE', #19722, #17417, #7886 ) ;
#23447 = ORIENTED_EDGE ( 'NONE', *, *, #12093, .T. ) ;
#23448 = FACE_OUTER_BOUND ( 'NONE', #15144, .T. ) ;
#23449 = CARTESIAN_POINT ( 'NONE',  ( 38.37017380507018771, -3.603840866421911038, 70.24448340153877268 ) ) ;
#23450 = EDGE_LOOP ( 'NONE', ( #15048, #6249, #25275, #1329, #21312, #2556, #10585, #10177, #19711, #18910, #24265, #17831, #24294, #11828, #11984, #16890 ) ) ;
#23451 = DIRECTION ( 'NONE',  ( 0.000000000000000000, -1.000000000000000000, 2.999999999999999839E-15 ) ) ;
#23452 = DIRECTION ( 'NONE',  ( 0.000000000000000000, -1.000000000000000000, 2.999999999999999839E-15 ) ) ;
#23453 = CARTESIAN_POINT ( 'NONE',  ( 36.98690846071097127, -11.80384086642191477, 69.45876917294175712 ) ) ;
#23454 = CARTESIAN_POINT ( 'NONE',  ( 35.56606138205697221, -5.022037326221718168, -5.474317061061731771 ) ) ;
#23455 = DIRECTION ( 'NONE',  ( 1.000000000000000000, -0.000000000000000000, 0.000000000000000000 ) ) ;
#23456 = CARTESIAN_POINT ( 'NONE',  ( 39.98359781491296161, -14.41368208888610525, 71.86517103874047052 ) ) ;
#23457 = CARTESIAN_POINT ( 'NONE',  ( 33.91905694501954116, 2.753407105083469197, 6.093960844037363600 ) ) ;
#23458 = VECTOR ( 'NONE', #19206, 999.9999999999998863 ) ;
#23459 = PLANE ( 'NONE',  #8940 ) ;
#23460 = VECTOR ( 'NONE', #5773, 1000.000000000000227 ) ;
#23461 = CARTESIAN_POINT ( 'NONE',  ( 43.31606138205700063, -13.43064139120327560, 11.56373968489310755 ) ) ;
#23462 = EDGE_CURVE ( 'NONE', #22022, #7686, #21011, .T. ) ;
#23463 = CARTESIAN_POINT ( 'NONE',  ( 37.80618814713138676, -1.703840866421908018, 69.62690120949091011 ) ) ;
#23464 = DIRECTION ( 'NONE',  ( -1.000000000000000000, 0.000000000000000000, 0.000000000000000000 ) ) ;
#23465 = CARTESIAN_POINT ( 'NONE',  ( 39.98359781491296161, -20.41368208888610525, 71.86517103874047052 ) ) ;
#23466 = DIRECTION ( 'NONE',  ( 0.000000000000000000, -2.999999999999999839E-15, -1.000000000000000000 ) ) ;
#23467 = CARTESIAN_POINT ( 'NONE',  ( 38.26194895904384907, -16.60384086642191548, 73.11602215082116629 ) ) ;
#23468 = DIRECTION ( 'NONE',  ( -1.000000000000000000, -2.999999999999999839E-15, 0.000000000000000000 ) ) ;
#23469 = CIRCLE ( 'NONE', #22251, 0.5000000000000004441 ) ;
#23470 = CARTESIAN_POINT ( 'NONE',  ( 38.93415946300897446, -16.11368208888611164, 73.09843995877329803 ) ) ;
#23471 = EDGE_LOOP ( 'NONE', ( #16424, #25274, #11902, #22834 ) ) ;
#23472 = CARTESIAN_POINT ( 'NONE',  ( 36.89935272106204422, -23.21368208888610241, 69.52238214136765748 ) ) ;
#23473 = VERTEX_POINT ( 'NONE', #934 ) ;
#23474 = CARTESIAN_POINT ( 'NONE',  ( 35.31606138205700773, -20.93319939328399926, 43.78741072286599945 ) ) ;
#23475 = CARTESIAN_POINT ( 'NONE',  ( 32.81606138205700773, 34.92314894770294131, 81.17823623207324601 ) ) ;
#23476 = VECTOR ( 'NONE', #4981, 1000.000000000000000 ) ;
#23477 = CARTESIAN_POINT ( 'NONE',  ( 37.69225076346193504, -23.80384086642191477, 70.42958956619166599 ) ) ;
#23478 = ORIENTED_EDGE ( 'NONE', *, *, #8040, .T. ) ;
#23479 = ORIENTED_EDGE ( 'NONE', *, *, #15066, .F. ) ;
#23480 = FACE_OUTER_BOUND ( 'NONE', #5623, .T. ) ;
#23481 = CARTESIAN_POINT ( 'NONE',  ( 33.56606138205700773, 42.19123852234595518, 61.30501292736988006 ) ) ;
#23482 = VERTEX_POINT ( 'NONE', #3354 ) ;
#23483 = CARTESIAN_POINT ( 'NONE',  ( 40.52078840805429394, -27.00384086642191761, 72.15350918040381600 ) ) ;
#23484 = CARTESIAN_POINT ( 'NONE',  ( 37.61123632939165873, 0.08631791111389161553, 73.73360434286902887 ) ) ;
#23485 = CYLINDRICAL_SURFACE ( 'NONE', #20076, 1.500000000000001332 ) ;
#23486 = ORIENTED_EDGE ( 'NONE', *, *, #7856, .F. ) ;
#23487 = ADVANCED_FACE ( 'NONE', ( #9305 ), #17147, .T. ) ;
#23488 = ORIENTED_EDGE ( 'NONE', *, *, #12078, .F. ) ;
#23489 = EDGE_CURVE ( 'NONE', #23228, #8670, #17274, .T. ) ;
#23490 = DIRECTION ( 'NONE',  ( -1.000000000000000000, 0.000000000000000000, 0.000000000000000000 ) ) ;
#23491 = CARTESIAN_POINT ( 'NONE',  ( 32.56606138205700773, 41.63025572888945192, 83.79244979444629848 ) ) ;
#23492 = EDGE_CURVE ( 'NONE', #17658, #19678, #15331, .T. ) ;
#23493 = CARTESIAN_POINT ( 'NONE',  ( 37.80618814713138676, -19.70384086642190624, 69.62690120949091011 ) ) ;
#23494 = DIRECTION ( 'NONE',  ( -1.000000000000000000, 1.301042606982604506E-30, 4.336808689942015271E-16 ) ) ;
#23495 = VECTOR ( 'NONE', #10513, 1000.000000000000227 ) ;
#23496 = ORIENTED_EDGE ( 'NONE', *, *, #17052, .F. ) ;
#23497 = CARTESIAN_POINT ( 'NONE',  ( 43.31606138205700063, -5.204193249396277032, 83.30501292736992980 ) ) ;
#23498 = FACE_OUTER_BOUND ( 'NONE', #3654, .T. ) ;
#23499 = DIRECTION ( 'NONE',  ( -1.219254108801168961E-15, 0.4425581086832399147, -0.8967398287344627850 ) ) ;
#23500 = CARTESIAN_POINT ( 'NONE',  ( 39.41296390513587511, -7.203840866421913347, 71.08074471024443142 ) ) ;
#23501 = ORIENTED_EDGE ( 'NONE', *, *, #19801, .T. ) ;
#23502 = EDGE_CURVE ( 'NONE', #1147, #23852, #21771, .T. ) ;
#23503 = CARTESIAN_POINT ( 'NONE',  ( 35.64099152588523367, -8.167181138186998979, 88.30501292736998664 ) ) ;
#23504 = VERTEX_POINT ( 'NONE', #5805 ) ;
#23505 = ORIENTED_EDGE ( 'NONE', *, *, #14826, .T. ) ;
#23506 = LINE ( 'NONE', #21328, #13083 ) ;
#23507 = CARTESIAN_POINT ( 'NONE',  ( 37.89291511884476904, -15.11368208888610098, 70.26206559358661252 ) ) ;
#23508 = CARTESIAN_POINT ( 'NONE',  ( 39.24876120206128860, -8.713682088886100630, 70.63227792289247020 ) ) ;
#23509 = ORIENTED_EDGE ( 'NONE', *, *, #14386, .T. ) ;
#23510 = ORIENTED_EDGE ( 'NONE', *, *, #3205, .F. ) ;
#23511 = DIRECTION ( 'NONE',  ( 1.000000000000000000, -5.510910596163088391E-31, -1.836970198721029688E-16 ) ) ;
#23512 = LINE ( 'NONE', #9636, #904 ) ;
#23513 = EDGE_LOOP ( 'NONE', ( #2885, #25133, #20922, #1227 ) ) ;
#23514 = DIRECTION ( 'NONE',  ( -9.027796614315171564E-31, -1.000000000000000000, -1.163336342344335610E-15 ) ) ;
#23515 = CARTESIAN_POINT ( 'NONE',  ( 37.69796330110505522, -14.50384086642191583, 73.09843995877329803 ) ) ;
#23516 = CIRCLE ( 'NONE', #13255, 3.000000000000002665 ) ;
#23517 = CARTESIAN_POINT ( 'NONE',  ( 42.56606138205700063, 2.740850673309605412, 6.112030963703427133 ) ) ;
#23518 =( GEOMETRIC_REPRESENTATION_CONTEXT ( 3 ) GLOBAL_UNCERTAINTY_ASSIGNED_CONTEXT ( ( #438 ) ) GLOBAL_UNIT_ASSIGNED_CONTEXT ( ( #6854, #13049, #20643 ) ) REPRESENTATION_CONTEXT ( 'NONE', 'WORKASPACE' ) );
#23519 = CARTESIAN_POINT ( 'NONE',  ( 32.81606138205700773, 41.44123852234595518, 61.30501292736988006 ) ) ;
#23520 = CARTESIAN_POINT ( 'NONE',  ( 37.60469502381300089, -19.21368208888609885, 70.49320253461759478 ) ) ;
#23521 = EDGE_LOOP ( 'NONE', ( #18788, #10626, #19249, #2688 ) ) ;
#23522 = ORIENTED_EDGE ( 'NONE', *, *, #15365, .F. ) ;
#23523 = LINE ( 'NONE', #3692, #21531 ) ;
#23524 = CARTESIAN_POINT ( 'NONE',  ( 38.26194895904383486, -17.01368208888610312, 69.64448340153877837 ) ) ;
#23525 = DIRECTION ( 'NONE',  ( 1.157642374584902751E-15, -0.3934158747763039088, 0.9193606199277819524 ) ) ;
#23526 = CARTESIAN_POINT ( 'NONE',  ( 41.81606138205697221, -3.103162021984027241, -5.046558096268735305 ) ) ;
#23527 = CARTESIAN_POINT ( 'NONE',  ( 38.82593461698262871, -28.91368208888610525, 69.62690120949091011 ) ) ;
#23528 = CARTESIAN_POINT ( 'NONE',  ( 40.64099152588522657, 40.83281886181300280, 79.30501292736983032 ) ) ;
#23529 = VECTOR ( 'NONE', #15539, 1000.000000000000000 ) ;
#23530 = AXIS2_PLACEMENT_3D ( 'NONE', #11861, #2042, #15829 ) ;
#23531 = DIRECTION ( 'NONE',  ( 1.000000000000000000, 3.491481338843134144E-15, -3.540251991789504463E-16 ) ) ;
#23532 = VERTEX_POINT ( 'NONE', #15457 ) ;
#23533 = ADVANCED_FACE ( 'NONE', ( #6057 ), #7478, .T. ) ;
#23534 = VECTOR ( 'NONE', #24535, 1000.000000000000114 ) ;
#23535 = DIRECTION ( 'NONE',  ( 1.000000000000000000, 2.805550545906363219E-15, -9.596449257708877207E-17 ) ) ;
#23536 = ORIENTED_EDGE ( 'NONE', *, *, #13440, .T. ) ;
#23537 = EDGE_LOOP ( 'NONE', ( #11064, #4178, #1767, #14123 ) ) ;
#23538 = CARTESIAN_POINT ( 'NONE',  ( 37.50301148336529877, -4.503840866421918498, 73.69843995877330656 ) ) ;
#23539 = VERTEX_POINT ( 'NONE', #4129 ) ;
#23540 = AXIS2_PLACEMENT_3D ( 'NONE', #9540, #7861, #25218 ) ;
#23541 = DIRECTION ( 'NONE',  ( 1.734723475976805122E-16, 3.491481338843134933E-15, 1.000000000000000000 ) ) ;
#23542 = CARTESIAN_POINT ( 'NONE',  ( 36.80608444377001121, -17.31368208888609672, 70.35351908239857721 ) ) ;
#23543 = ORIENTED_EDGE ( 'NONE', *, *, #19047, .T. ) ;
#23544 = CARTESIAN_POINT ( 'NONE',  ( 33.31606138205700773, -5.204193249396280585, 82.80501292736992980 ) ) ;
#23545 = FACE_OUTER_BOUND ( 'NONE', #9854, .T. ) ;
#23546 = CARTESIAN_POINT ( 'NONE',  ( 39.73277004305198545, -12.21368208888610951, 73.23812341099225875 ) ) ;
#23547 = VERTEX_POINT ( 'NONE', #21258 ) ;
#23548 = VECTOR ( 'NONE', #14634, 1000.000000000000114 ) ;
#23549 = EDGE_CURVE ( 'NONE', #18450, #12829, #13533, .T. ) ;
#23550 = DIRECTION ( 'NONE',  ( 2.792262043613788535E-15, -0.8967398287344627850, -0.4425581086832399147 ) ) ;
#23551 = CARTESIAN_POINT ( 'NONE',  ( 0.000000000000000000, 2.823374736507280597E-13, 81.37823623207336254 ) ) ;
#23552 = EDGE_CURVE ( 'NONE', #30, #3261, #5549, .T. ) ;
#23553 = CIRCLE ( 'NONE', #102, 0.7106531558045068309 ) ;
#23554 = EDGE_CURVE ( 'NONE', #1986, #4892, #11485, .T. ) ;
#23555 = DIRECTION ( 'NONE',  ( 0.000000000000000000, 0.7540134720837717852, 0.6568589528324747517 ) ) ;
#23556 = EDGE_CURVE ( 'NONE', #12192, #17722, #17533, .T. ) ;
#23557 = SURFACE_STYLE_FILL_AREA ( #3721 ) ;
#23558 = LINE ( 'NONE', #12119, #22150 ) ;
#23559 = TOROIDAL_SURFACE ( 'NONE', #12486, 1.800000000000000044, 0.2000000000000000111 ) ;
#23560 = CARTESIAN_POINT ( 'NONE',  ( 43.31606138205700063, -1.963190818658398173, 19.89143565483009013 ) ) ;
#23561 = CARTESIAN_POINT ( 'NONE',  ( 39.41296390513587511, -15.20384086642191157, 71.08074471024441721 ) ) ;
#23562 = CARTESIAN_POINT ( 'NONE',  ( 38.00113996487114321, -27.91368208888610170, 72.53360434286901182 ) ) ;
#23563 = ORIENTED_EDGE ( 'NONE', *, *, #10192, .F. ) ;
#23564 = CARTESIAN_POINT ( 'NONE',  ( 40.31606138205700773, -20.32227907754186802, 76.00185088427946312 ) ) ;
#23565 = EDGE_CURVE ( 'NONE', #15554, #17064, #9898, .T. ) ;
#23566 = AXIS2_PLACEMENT_3D ( 'NONE', #3397, #7780, #11654 ) ;
#23567 = CARTESIAN_POINT ( 'NONE',  ( 36.31606138205700063, 5.691238522346998785, 68.80501292736998664 ) ) ;
#23568 = ORIENTED_EDGE ( 'NONE', *, *, #1761, .T. ) ;
#23569 = ORIENTED_EDGE ( 'NONE', *, *, #23166, .F. ) ;
#23570 = CIRCLE ( 'NONE', #8380, 0.5000000000000004441 ) ;
#23571 = CARTESIAN_POINT ( 'NONE',  ( 39.82603832034400426, 0.6961591335780910050, 70.35351908239860563 ) ) ;
#23572 = VECTOR ( 'NONE', #16804, 1000.000000000000000 ) ;
#23573 = CARTESIAN_POINT ( 'NONE',  ( 37.38336156205274818, -21.71368208888610241, 72.12822762946750288 ) ) ;
#23574 = CARTESIAN_POINT ( 'NONE',  ( 40.55423172469004811, -0.4136820888861054146, 72.05058123536544201 ) ) ;
#23575 = EDGE_LOOP ( 'NONE', ( #15660, #13861, #15434, #18750 ) ) ;
#23576 = CARTESIAN_POINT ( 'NONE',  ( 38.31606138205700063, 16.19123852234700678, 71.30501292736995822 ) ) ;
#23577 = CARTESIAN_POINT ( 'NONE',  ( 39.95015449827720744, -27.00384086642191050, 71.96809898377885872 ) ) ;
#23578 = CARTESIAN_POINT ( 'NONE',  ( 36.31606138205700063, -29.30876147765401640, 69.30501292737010033 ) ) ;
#23579 = ORIENTED_EDGE ( 'NONE', *, *, #13196, .T. ) ;
#23580 = AXIS2_PLACEMENT_3D ( 'NONE', #24486, #22451, #20395 ) ;
#23581 = DIRECTION ( 'NONE',  ( 1.000000000000000000, 2.751104698760144965E-15, -1.228345504986739201E-16 ) ) ;
#23582 = DIRECTION ( 'NONE',  ( 0.000000000000000000, 0.7540134720837716742, 0.6568589528324746407 ) ) ;
#23583 = CARTESIAN_POINT ( 'NONE',  ( 40.52078840805429394, -11.00384086642191406, 72.15350918040385864 ) ) ;
#23584 = CARTESIAN_POINT ( 'NONE',  ( 44.06606138205700063, 40.39281886181299797, 82.55501292736983032 ) ) ;
#23585 =( NAMED_UNIT ( * ) SI_UNIT ( $, .STERADIAN. ) SOLID_ANGLE_UNIT ( ) );
#23586 = PRESENTATION_LAYER_ASSIGNMENT (  '', '', ( #5508 ) ) ;
#23587 = CARTESIAN_POINT ( 'NONE',  ( 36.68196826583682935, -13.61368208888610454, 71.96809898377888715 ) ) ;
#23588 = LINE ( 'NONE', #23710, #13058 ) ;
#23589 = CARTESIAN_POINT ( 'NONE',  ( 38.82593461698262871, -24.91368208888610170, 69.62690120949091011 ) ) ;
#23590 = VECTOR ( 'NONE', #16242, 1000.000000000000000 ) ;
#23591 = EDGE_CURVE ( 'NONE', #5873, #19839, #17271, .T. ) ;
#23592 = EDGE_CURVE ( 'NONE', #17862, #9175, #1657, .T. ) ;
#23593 = CARTESIAN_POINT ( 'NONE',  ( 37.31606138205702194, -20.92507021039840254, 32.39841118875936132 ) ) ;
#23594 = VECTOR ( 'NONE', #17931, 1000.000000000000000 ) ;
#23595 = CARTESIAN_POINT ( 'NONE',  ( 36.68196826583682935, -2.003840866421909617, 70.79240656858108593 ) ) ;
#23596 = CONTEXT_DEPENDENT_SHAPE_REPRESENTATION ( #21486, #6181 ) ;
#23597 = LINE ( 'NONE', #2450, #23159 ) ;
#23598 = CARTESIAN_POINT ( 'NONE',  ( 39.38009889167650357, -20.21368208888610951, 72.75271321436731853 ) ) ;
#23599 = DIRECTION ( 'NONE',  ( -1.734723475976805122E-16, -3.491481338843134933E-15, -1.000000000000000000 ) ) ;
#23600 = CIRCLE ( 'NONE', #9231, 4.000000000000003553 ) ;
#23601 = ADVANCED_FACE ( 'NONE', ( #7736 ), #3992, .F. ) ;
#23602 = CARTESIAN_POINT ( 'NONE',  ( 39.98359781491296161, -17.20384086642190979, 70.89533451361945993 ) ) ;
#23603 = DIRECTION ( 'NONE',  ( 0.000000000000000000, 0.5706330172266920187, -0.8212051873014210024 ) ) ;
#23604 = MECHANICAL_DESIGN_GEOMETRIC_PRESENTATION_REPRESENTATION (  '', ( #25242 ), #4291 ) ;
#23605 = CARTESIAN_POINT ( 'NONE',  ( 39.98359781491296161, -10.41368208888610347, 71.86517103874048473 ) ) ;
#23606 = EDGE_LOOP ( 'NONE', ( #4417, #14917, #18294, #3120 ) ) ;
#23607 = CARTESIAN_POINT ( 'NONE',  ( 36.36258059203031934, -23.71368208888610951, 72.86986841596734621 ) ) ;
#23608 = EDGE_LOOP ( 'NONE', ( #19625, #21938, #9025, #16376 ) ) ;
#23609 = CARTESIAN_POINT ( 'NONE',  ( 30.81606138205696865, -3.227578639999848509, -4.500312080287595329 ) ) ;
#23610 = VECTOR ( 'NONE', #14171, 1000.000000000000000 ) ;
#23611 = LINE ( 'NONE', #7401, #19886 ) ;
#23612 = CARTESIAN_POINT ( 'NONE',  ( 38.26194895904384197, -24.60384086642190837, 72.51602215082114355 ) ) ;
#23613 = VECTOR ( 'NONE', #6962, 1000.000000000000000 ) ;
#23614 = VERTEX_POINT ( 'NONE', #13662 ) ;
#23615 = ADVANCED_FACE ( 'NONE', ( #15715 ), #17399, .F. ) ;
#23616 = ORIENTED_EDGE ( 'NONE', *, *, #5103, .T. ) ;
#23617 = LINE ( 'NONE', #21564, #8016 ) ;
#23618 = AXIS2_PLACEMENT_3D ( 'NONE', #25079, #7464, #13398 ) ;
#23619 = DIRECTION ( 'NONE',  ( 0.000000000000000000, -0.3299742535180970049, 0.9439899321577400748 ) ) ;
#23620 = ORIENTED_EDGE ( 'NONE', *, *, #8560, .T. ) ;
#23621 = CARTESIAN_POINT ( 'NONE',  ( 31.81606138205700418, -34.55876147765410167, 66.30501292737000085 ) ) ;
#23622 = CARTESIAN_POINT ( 'NONE',  ( 40.14115730948191185, 0.8961591335780898504, 71.43714994484035685 ) ) ;
#23623 =( BOUNDED_CURVE ( )  B_SPLINE_CURVE ( 3, ( #19878, #2217, #14330, #10097 ),
 .UNSPECIFIED., .F., .T. ) 
 B_SPLINE_CURVE_WITH_KNOTS ( ( 4, 4 ),
 ( 1.570796326794895004, 3.141592653589795336 ),
 .UNSPECIFIED. ) 
 CURVE ( )  GEOMETRIC_REPRESENTATION_ITEM ( )  RATIONAL_B_SPLINE_CURVE ( ( 1.000000000000000000, 0.8047378541243649375, 0.8047378541243649375, 1.000000000000000000 ) ) 
 REPRESENTATION_ITEM ( '' )  );
#23624 = PLANE ( 'NONE',  #19519 ) ;
#23625 = CARTESIAN_POINT ( 'NONE',  ( 40.77203464402485622, -4.513682088886104893, 71.32335560751961623 ) ) ;
#23626 = DIRECTION ( 'NONE',  ( -1.000000000000000000, -0.000000000000000000, 0.000000000000000000 ) ) ;
#23627 = ORIENTED_EDGE ( 'NONE', *, *, #66, .T. ) ;
#23628 = EDGE_LOOP ( 'NONE', ( #15139, #10368, #13390, #16815 ) ) ;
#23629 = APPLICATION_CONTEXT ( 'automotive_design' ) ;
#23630 = DIRECTION ( 'NONE',  ( 1.000000000000000000, -6.018531076210110289E-31, -1.734723475976804876E-16 ) ) ;
#23631 = DIRECTION ( 'NONE',  ( 1.000000000000000000, 0.000000000000000000, 0.000000000000000000 ) ) ;
#23632 = CARTESIAN_POINT ( 'NONE',  ( 40.14115730948191185, -21.10384086642191193, 71.43714994484031422 ) ) ;
#23633 = LINE ( 'NONE', #10621, #22345 ) ;
#23634 = ORIENTED_EDGE ( 'NONE', *, *, #23270, .F. ) ;
#23635 = LINE ( 'NONE', #9862, #2011 ) ;
#23636 = CARTESIAN_POINT ( 'NONE',  ( 32.81606138205700773, 32.99511671078946762, 63.14259751872857152 ) ) ;
#23637 = EDGE_LOOP ( 'NONE', ( #7312, #1005, #455, #20470 ) ) ;
#23638 = CARTESIAN_POINT ( 'NONE',  ( 37.69225076346193504, -7.803840866421912104, 70.42958956619168021 ) ) ;
#23639 = FACE_OUTER_BOUND ( 'NONE', #1596, .T. ) ;
#23640 = EDGE_LOOP ( 'NONE', ( #13739, #17842, #24969, #7522 ) ) ;
#23641 = CARTESIAN_POINT ( 'NONE',  ( 31.91606138205697363, -4.349482454670880571, -5.142398479549302515 ) ) ;
#23642 = VERTEX_POINT ( 'NONE', #19446 ) ;
#23643 = ORIENTED_EDGE ( 'NONE', *, *, #5700, .T. ) ;
#23645 = EDGE_CURVE ( 'NONE', #2401, #24395, #1792, .T. ) ;
#23644 = LINE ( 'NONE', #5875, #24156 ) ;
#23646 = CARTESIAN_POINT ( 'NONE',  ( 38.63098279924288647, -10.91368208888610170, 70.22690120949091863 ) ) ;
#23647 = ADVANCED_FACE ( 'NONE', ( #19578 ), #118, .F. ) ;
#23648 = CARTESIAN_POINT ( 'NONE',  ( 38.63098279924288647, -12.91368208888610525, 70.22690120949090442 ) ) ;
#23649 = ORIENTED_EDGE ( 'NONE', *, *, #19178, .F. ) ;
#23650 = ADVANCED_FACE ( 'NONE', ( #19704 ), #8002, .T. ) ;
#23651 = EDGE_LOOP ( 'NONE', ( #204, #7853 ) ) ;
#23652 = LINE ( 'NONE', #9755, #4570 ) ;
#23653 = CARTESIAN_POINT ( 'NONE',  ( 43.06606138205700063, 41.44123852234595518, 61.30501292736988006 ) ) ;
#23654 = ORIENTED_EDGE ( 'NONE', *, *, #3502, .F. ) ;
#23655 = FACE_OUTER_BOUND ( 'NONE', #10253, .T. ) ;
#23656 = CARTESIAN_POINT ( 'NONE',  ( 37.25202387243754032, -16.40384086642191619, 72.75271321436731853 ) ) ;
#23657 = AXIS2_PLACEMENT_3D ( 'NONE', #15216, #13042, #7243 ) ;
#23658 = CARTESIAN_POINT ( 'NONE',  ( 44.81606138205700063, -24.55876147765401285, 70.30501292737008612 ) ) ;
#23659 = LINE ( 'NONE', #6015, #8824 ) ;
#23660 = CARTESIAN_POINT ( 'NONE',  ( 39.41296390513587511, -20.41368208888610170, 71.67976084211551324 ) ) ;
#23661 = ORIENTED_EDGE ( 'NONE', *, *, #9151, .F. ) ;
#23662 = ORIENTED_EDGE ( 'NONE', *, *, #7512, .T. ) ;
#23663 = CARTESIAN_POINT ( 'NONE',  ( 41.06606138205703616, -24.72749677399387380, 32.19456755146972426 ) ) ;
#23664 = CARTESIAN_POINT ( 'NONE',  ( 39.95015449827720744, -12.61368208888610454, 70.79240656858105751 ) ) ;
#23665 = EDGE_CURVE ( 'NONE', #11300, #6883, #4382, .T. ) ;
#23666 = DIRECTION ( 'NONE',  ( 0.000000000000000000, -0.8212051873014208914, -0.5706330172266919076 ) ) ;
#23667 = DIRECTION ( 'NONE',  ( -1.734723475976804876E-16, -3.552713678800500140E-15, -1.000000000000000000 ) ) ;
#23668 = CARTESIAN_POINT ( 'NONE',  ( 32.81606138205700773, 2.191238522347000117, 69.30501292737000085 ) ) ;
#23669 = DIRECTION ( 'NONE',  ( 2.792262043613788535E-15, -0.8967398287344627850, -0.4425581086832398592 ) ) ;
#23670 = CIRCLE ( 'NONE', #11345, 0.7500000000000006661 ) ;
#23671 = DIRECTION ( 'NONE',  ( 0.000000000000000000, -0.7516416929448823669, -0.6595716529892345914 ) ) ;
#23672 = DIRECTION ( 'NONE',  ( 0.000000000000000000, -0.7516416929448760387, -0.6595716529892418079 ) ) ;
#23673 = ORIENTED_EDGE ( 'NONE', *, *, #24642, .F. ) ;
#23674 = ORIENTED_EDGE ( 'NONE', *, *, #24985, .F. ) ;
#23675 = CARTESIAN_POINT ( 'NONE',  ( 36.29569395875881099, -4.303840866421919209, 72.77780686321129622 ) ) ;
#23676 = ORIENTED_EDGE ( 'NONE', *, *, #12903, .F. ) ;
#23677 = DIRECTION ( 'NONE',  ( 1.327674326049700866E-15, -0.4425581086832336419, 0.8967398287344658936 ) ) ;
#23678 = CARTESIAN_POINT ( 'NONE',  ( 40.14115730948191185, -8.513682088886104893, 71.32335560751961623 ) ) ;
#23679 = VERTEX_POINT ( 'NONE', #2428 ) ;
#23680 = DIRECTION ( 'NONE',  ( 0.000000000000000000, -1.000000000000000000, 2.775557561562891351E-15 ) ) ;
#23681 = CARTESIAN_POINT ( 'NONE',  ( 39.02088643472237095, -16.91368208888609814, 69.02690120949091579 ) ) ;
#23682 = SURFACE_STYLE_FILL_AREA ( #15827 ) ;
#23683 = CYLINDRICAL_SURFACE ( 'NONE', #10412, 0.4999999999999943379 ) ;
#23684 = EDGE_CURVE ( 'NONE', #20897, #4191, #9072, .T. ) ;
#23685 = CARTESIAN_POINT ( 'NONE',  ( 44.81606138205700063, -34.55876147765410167, 70.30501292737000085 ) ) ;
#23686 = DIRECTION ( 'NONE',  ( 0.000000000000000000, 0.3299742535180974490, -0.9439899321577398528 ) ) ;
#23687 = CARTESIAN_POINT ( 'NONE',  ( 45.81606138205705037, -30.65246816789533213, 72.44500581826358143 ) ) ;
#23688 = LINE ( 'NONE', #2675, #23806 ) ;
#23689 = CARTESIAN_POINT ( 'NONE',  ( 38.73920764526925353, -22.11368208888610098, 72.49843995877330372 ) ) ;
#23690 = ORIENTED_EDGE ( 'NONE', *, *, #18983, .F. ) ;
#23691 = CARTESIAN_POINT ( 'NONE',  ( 39.20536636138601949, -22.02780952473084852, 75.81186282291122325 ) ) ;
#23692 = DIRECTION ( 'NONE',  ( -1.000000000000000000, -2.999999999999999839E-15, 0.000000000000000000 ) ) ;
#23693 = ORIENTED_EDGE ( 'NONE', *, *, #9470, .F. ) ;
#23694 = ORIENTED_EDGE ( 'NONE', *, *, #7465, .T. ) ;
#23695 = CARTESIAN_POINT ( 'NONE',  ( 40.26954217208372455, -24.90384086642191619, 72.86986841596730358 ) ) ;
#23696 = CARTESIAN_POINT ( 'NONE',  ( 37.25260217561390874, -21.61368208888610098, 71.78268878715392987 ) ) ;
#23697 = PRODUCT ( 'Base Pivot Pin', 'Base Pivot Pin', '', ( #21167 ) ) ;
#23698 = CARTESIAN_POINT ( 'NONE',  ( 38.82593461698262871, -24.91368208888610170, 69.62690120949091011 ) ) ;
#23699 = ORIENTED_EDGE ( 'NONE', *, *, #9784, .F. ) ;
#23700 = CARTESIAN_POINT ( 'NONE',  ( 36.31606138205700063, -22.22127907754180853, 85.30501292736998664 ) ) ;
#23701 = CARTESIAN_POINT ( 'NONE',  ( 38.00113996487112189, -1.703840866421911571, 70.22690120949091863 ) ) ;
#23702 =( NAMED_UNIT ( * ) SI_UNIT ( $, .STERADIAN. ) SOLID_ANGLE_UNIT ( ) );
#23703 = ORIENTED_EDGE ( 'NONE', *, *, #714, .T. ) ;
#23704 = DIRECTION ( 'NONE',  ( -8.673617379884039170E-17, 1.163336342344335610E-15, -1.000000000000000000 ) ) ;
#23705 = CYLINDRICAL_SURFACE ( 'NONE', #16587, 1.250000000000001110 ) ;
#23706 = CARTESIAN_POINT ( 'NONE',  ( 38.37017380507018771, -5.603840866421911926, 69.04448340153881247 ) ) ;
#23707 = CARTESIAN_POINT ( 'NONE',  ( 35.31606138205700773, 2.715274261285174351, 65.05190033008260286 ) ) ;
#23708 = DIRECTION ( 'NONE',  ( 0.000000000000000000, -2.999999999999999839E-15, -1.000000000000000000 ) ) ;
#23709 = CARTESIAN_POINT ( 'NONE',  ( 36.80608444377001121, -5.313682088886100274, 70.35351908239860563 ) ) ;
#23710 = CARTESIAN_POINT ( 'NONE',  ( 36.31606138205700063, -12.76023008545320714, 21.53290024082827969 ) ) ;
#23711 = EDGE_CURVE ( 'NONE', #20407, #20277, #15636, .T. ) ;
#23712 = CARTESIAN_POINT ( 'NONE',  ( 39.38009889167650357, -28.21368208888610951, 72.75271321436730432 ) ) ;
#23713 = DIRECTION ( 'NONE',  ( 0.000000000000000000, -0.3299742535180969494, 0.9439899321577399638 ) ) ;
#23714 = CARTESIAN_POINT ( 'NONE',  ( 36.68196826583682935, -4.003840866421911393, 70.79240656858108593 ) ) ;
#23715 = CARTESIAN_POINT ( 'NONE',  ( 32.56606138205700773, 40.39281886181299797, 82.55501292736983032 ) ) ;
#23716 = CARTESIAN_POINT ( 'NONE',  ( 36.49096545463212493, -11.51368208888609956, 71.43714994484034264 ) ) ;
#23717 = LINE ( 'NONE', #6087, #14779 ) ;
#23718 = AXIS2_PLACEMENT_3D ( 'NONE', #20174, #12079, #6639 ) ;
#23719 = CARTESIAN_POINT ( 'NONE',  ( 36.80608444377001831, -14.30384086642191122, 72.40698646996135324 ) ) ;
#23720 = EDGE_CURVE ( 'NONE', #5143, #10110, #24070, .T. ) ;
#23721 = CARTESIAN_POINT ( 'NONE',  ( 43.31606138205700063, -22.22127907754180853, 85.30501292736998664 ) ) ;
#23722 = VECTOR ( 'NONE', #1850, 1000.000000000000000 ) ;
#23723 = AXIS2_PLACEMENT_3D ( 'NONE', #13694, #19872, #13815 ) ;
#23724 = EDGE_CURVE ( 'NONE', #22567, #12430, #492, .T. ) ;
#23725 = CARTESIAN_POINT ( 'NONE',  ( 40.14115730948191185, -12.51368208888610489, 71.32335560751960202 ) ) ;
#23726 = VERTEX_POINT ( 'NONE', #22402 ) ;
#23727 = CARTESIAN_POINT ( 'NONE',  ( 35.86008812008917346, -23.51368208888609956, 71.43714994484032843 ) ) ;
#23728 = ORIENTED_EDGE ( 'NONE', *, *, #18675, .T. ) ;
#23729 = CARTESIAN_POINT ( 'NONE',  ( 43.31606138205700063, -39.60075215179220720, 69.23691647014479145 ) ) ;
#23730 = LINE ( 'NONE', #11904, #14475 ) ;
#23731 = CARTESIAN_POINT ( 'NONE',  ( 39.41296390513587511, -15.20384086642191157, 71.08074471024441721 ) ) ;
#23732 = EDGE_CURVE ( 'NONE', #8708, #7878, #18168, .T. ) ;
#23733 = EDGE_CURVE ( 'NONE', #25254, #9967, #744, .T. ) ;
#23734 = VERTEX_POINT ( 'NONE', #2678 ) ;
#23735 = VERTEX_POINT ( 'NONE', #8501 ) ;
#23736 = CARTESIAN_POINT ( 'NONE',  ( 39.65578219934079840, -29.08214825217539712, 70.78045470424321195 ) ) ;
#23737 = CARTESIAN_POINT ( 'NONE',  ( 46.81606138205697221, -3.227578639999799659, -4.500312080287595329 ) ) ;
#23738 = CARTESIAN_POINT ( 'NONE',  ( 40.33642880535521869, -25.30384086642191477, 69.98269868914864844 ) ) ;
#23739 = CARTESIAN_POINT ( 'NONE',  ( 36.31606138205700063, 37.94123852234599781, 74.30501292736988717 ) ) ;
#23740 = CARTESIAN_POINT ( 'NONE',  ( 36.29569395875879678, 0.6863179111138985045, 69.98269868914869107 ) ) ;
#23741 = EDGE_CURVE ( 'NONE', #14213, #16039, #21897, .T. ) ;
#23742 = MECHANICAL_DESIGN_GEOMETRIC_PRESENTATION_REPRESENTATION (  '', ( #9371 ), #1135 ) ;
#23743 = ADVANCED_FACE ( 'NONE', ( #16334 ), #12377, .T. ) ;
#23744 = ORIENTED_EDGE ( 'NONE', *, *, #18319, .F. ) ;
#23745 = ORIENTED_EDGE ( 'NONE', *, *, #14555, .T. ) ;
#23746 = AXIS2_PLACEMENT_3D ( 'NONE', #20787, #4801, #8819 ) ;
#23747 = CIRCLE ( 'NONE', #5260, 2.999999999999998668 ) ;
#23748 = CYLINDRICAL_SURFACE ( 'NONE', #21951, 1.750000000000001554 ) ;
#23749 = CARTESIAN_POINT ( 'NONE',  ( 40.56606138205697931, -5.948051402551118194, 9.959574150503843981 ) ) ;
#23750 = CARTESIAN_POINT ( 'NONE',  ( 39.38009889167648936, -19.40384086642190908, 70.00779233799262613 ) ) ;
#23751 = FACE_OUTER_BOUND ( 'NONE', #21141, .T. ) ;
#23752 = ORIENTED_EDGE ( 'NONE', *, *, #16642, .F. ) ;
#23753 = CARTESIAN_POINT ( 'NONE',  ( 33.31606138205700773, 1.535676793533870210, 63.36117568837578062 ) ) ;
#23754 = CARTESIAN_POINT ( 'NONE',  ( 31.81606138205700418, 2.788239579249953820E-13, 80.37823623207336254 ) ) ;
#23755 = ORIENTED_EDGE ( 'NONE', *, *, #625, .T. ) ;
#23756 = CARTESIAN_POINT ( 'NONE',  ( 38.73920764526923932, -5.503840866421911393, 70.26206559358664094 ) ) ;
#23757 = CARTESIAN_POINT ( 'NONE',  ( 38.14273442609844977, -33.30876147765400219, 70.32014858831730919 ) ) ;
#23758 = VERTEX_POINT ( 'NONE', #22271 ) ;
#23759 = CARTESIAN_POINT ( 'NONE',  ( 31.91606138205697718, -5.918777154956192277, -5.916875169744970187 ) ) ;
#23760 = EDGE_LOOP ( 'NONE', ( #19917, #18887, #18271, #2121 ) ) ;
#23761 = ORIENTED_EDGE ( 'NONE', *, *, #16177, .F. ) ;
#23762 = CIRCLE ( 'NONE', #9803, 10.00000000000000178 ) ;
#23763 = CARTESIAN_POINT ( 'NONE',  ( 39.31606138205700063, 43.19123852234595518, 61.30501292736988006 ) ) ;
#23764 = CARTESIAN_POINT ( 'NONE',  ( 39.51027997493896748, -6.513682088886100452, 71.32335560751961623 ) ) ;
#23765 = VECTOR ( 'NONE', #6234, 1000.000000000000000 ) ;
#23766 = AXIS2_PLACEMENT_3D ( 'NONE', #9615, #11158, #24782 ) ;
#23767 = CARTESIAN_POINT ( 'NONE',  ( 39.51027997493896748, -4.513682088886101340, 71.32335560751961623 ) ) ;
#23768 = EDGE_LOOP ( 'NONE', ( #19053, #4702, #22972, #12098 ) ) ;
#23769 = ORIENTED_EDGE ( 'NONE', *, *, #4566, .F. ) ;
#23770 = CARTESIAN_POINT ( 'NONE',  ( 39.31606138205700063, 42.19123852234599781, 75.30501292736987295 ) ) ;
#23771 = CARTESIAN_POINT ( 'NONE',  ( 44.81606138205700063, -34.55876147765401640, 70.30501292737011454 ) ) ;
#23772 = VERTEX_POINT ( 'NONE', #6315 ) ;
#23773 = DIRECTION ( 'NONE',  ( -1.000000000000000000, -2.602085213965208275E-15, 0.000000000000000000 ) ) ;
#23774 = CARTESIAN_POINT ( 'NONE',  ( 39.38009889167648936, -19.40384086642190908, 70.00779233799262613 ) ) ;
#23775 = DIRECTION ( 'NONE',  ( 0.000000000000000000, 1.000000000000000000, -2.999999999999999839E-15 ) ) ;
#23776 = CARTESIAN_POINT ( 'NONE',  ( 36.81606138205700063, -0.7263636227174442572, 61.39059882987834982 ) ) ;
#23777 = CARTESIAN_POINT ( 'NONE',  ( 39.31606138205700063, 43.19123852234599070, 73.55501292736987295 ) ) ;
#23778 = ORIENTED_EDGE ( 'NONE', *, *, #22042, .F. ) ;
#23779 = ORIENTED_EDGE ( 'NONE', *, *, #20775, .F. ) ;
#23780 = CARTESIAN_POINT ( 'NONE',  ( 43.31606138205698642, -7.467730535347520515, -2.778285769174305919 ) ) ;
#23781 = CARTESIAN_POINT ( 'NONE',  ( 37.25202387243752611, -15.21368208888610063, 70.00779233799262613 ) ) ;
#23782 = DIRECTION ( 'NONE',  ( -1.510383499235849534E-16, -0.1218693434051499741, -0.9925461516413217611 ) ) ;
#23783 = AXIS2_PLACEMENT_3D ( 'NONE', #14514, #11168, #24665 ) ;
#23784 = FACE_BOUND ( 'NONE', #23441, .T. ) ;
#23785 = CARTESIAN_POINT ( 'NONE',  ( 33.57054761034910229, 3.412271088041349820, 6.349711998884802533 ) ) ;
#23786 = DIRECTION ( 'NONE',  ( -1.000000000000000000, -2.777772052464415468E-15, 1.096737058023870976E-16 ) ) ;
#23787 = CARTESIAN_POINT ( 'NONE',  ( 45.81606138205700063, 46.92314894770293421, 79.37823623207319201 ) ) ;
#23788 = DIRECTION ( 'NONE',  ( -1.000000000000000000, 0.000000000000000000, 0.000000000000000000 ) ) ;
#23789 = VERTEX_POINT ( 'NONE', #8246 ) ;
#23790 = DIRECTION ( 'NONE',  ( 0.000000000000000000, -1.000000000000000000, 3.491481338843135327E-15 ) ) ;
#23791 = ORIENTED_EDGE ( 'NONE', *, *, #12474, .T. ) ;
#23792 = ORIENTED_EDGE ( 'NONE', *, *, #15572, .T. ) ;
#23793 = CARTESIAN_POINT ( 'NONE',  ( 39.12911128074872380, -3.503840866421911393, 69.06206559358666652 ) ) ;
#23794 = AXIS2_PLACEMENT_3D ( 'NONE', #15499, #7409, #19373 ) ;
#23795 = ORIENTED_EDGE ( 'NONE', *, *, #18408, .F. ) ;
#23796 = CARTESIAN_POINT ( 'NONE',  ( 40.31606138205700773, -12.87480755223282713, 20.78922580900563588 ) ) ;
#23797 = CARTESIAN_POINT ( 'NONE',  ( 37.69796330110504101, -7.113682088886100985, 69.66206559358663242 ) ) ;
#23798 = VECTOR ( 'NONE', #19902, 1000.000000000000227 ) ;
#23799 = ORIENTED_EDGE ( 'NONE', *, *, #9274, .F. ) ;
#23800 = DIRECTION ( 'NONE',  ( 0.000000000000000000, -1.000000000000000000, 3.325260651745651169E-15 ) ) ;
#23801 = CARTESIAN_POINT ( 'NONE',  ( 35.86008812008917346, -13.51368208888610667, 71.43714994484034264 ) ) ;
#23802 = CARTESIAN_POINT ( 'NONE',  ( 43.27472635360392417, 2.989809604489832573, 6.109225132705429218 ) ) ;
#23803 = PLANE ( 'NONE',  #93 ) ;
#23804 = EDGE_CURVE ( 'NONE', #14470, #20311, #19969, .T. ) ;
#23805 = DIRECTION ( 'NONE',  ( -1.067465804653198538E-15, 0.4425581086832399147, -0.8967398287344627850 ) ) ;
#23806 = VECTOR ( 'NONE', #6053, 1000.000000000000000 ) ;
#23807 = ADVANCED_FACE ( 'NONE', ( #6438 ), #14178, .T. ) ;
#23808 = FACE_OUTER_BOUND ( 'NONE', #452, .T. ) ;
#23809 = DIRECTION ( 'NONE',  ( 0.000000000000000000, 1.000000000000000000, 0.000000000000000000 ) ) ;
#23810 = DIRECTION ( 'NONE',  ( 0.000000000000000000, 0.6568589528324746407, -0.7540134720837717852 ) ) ;
#23811 = CARTESIAN_POINT ( 'NONE',  ( 38.63098279924288647, -26.91368208888610170, 70.22690120949089021 ) ) ;
#23812 = VECTOR ( 'NONE', #6971, 1000.000000000000000 ) ;
#23813 = EDGE_LOOP ( 'NONE', ( #16279, #14240, #1681, #4737 ) ) ;
#23814 = CARTESIAN_POINT ( 'NONE',  ( 39.82744760895728575, -21.57230399584641845, 75.83179758371670687 ) ) ;
#23815 = CARTESIAN_POINT ( 'NONE',  ( 30.81606138205700418, -39.60718113818700203, 84.30501292737011454 ) ) ;
#23816 = ORIENTED_EDGE ( 'NONE', *, *, #10810, .F. ) ;
#23817 = ORIENTED_EDGE ( 'NONE', *, *, #16105, .T. ) ;
#23818 = CARTESIAN_POINT ( 'NONE',  ( 40.26954217208372455, -22.90384086642191974, 72.86986841596734621 ) ) ;
#23819 = VECTOR ( 'NONE', #18290, 1000.000000000000000 ) ;
#23820 = EDGE_CURVE ( 'NONE', #981, #14083, #22021, .T. ) ;
#23821 = CARTESIAN_POINT ( 'NONE',  ( 37.80618814713140097, -27.91368208888610880, 73.13360434286902034 ) ) ;
#23822 = DIRECTION ( 'NONE',  ( 1.000000000000000000, 0.000000000000000000, 0.000000000000000000 ) ) ;
#23823 = VECTOR ( 'NONE', #22077, 1000.000000000000000 ) ;
#23824 = CYLINDRICAL_SURFACE ( 'NONE', #17622, 1.000000000000000888 ) ;
#23825 = ORIENTED_EDGE ( 'NONE', *, *, #13592, .F. ) ;
#23826 = CARTESIAN_POINT ( 'NONE',  ( 40.31606138205699352, -10.17000407126883488, 36.59108960988216808 ) ) ;
#23827 = DIRECTION ( 'NONE',  ( 1.327674326049719602E-15, -0.4425581086832399147, 0.8967398287344627850 ) ) ;
#23828 = CARTESIAN_POINT ( 'NONE',  ( 40.55423172469004101, -3.203840866421916456, 70.70992431699450265 ) ) ;
#23829 = CYLINDRICAL_SURFACE ( 'NONE', #15228, 0.5000000000000004441 ) ;
#23830 = AXIS2_PLACEMENT_3D ( 'NONE', #10808, #20596, #8629 ) ;
#23831 = CYLINDRICAL_SURFACE ( 'NONE', #3347, 1.000000000000000888 ) ;
#23832 = CARTESIAN_POINT ( 'NONE',  ( 39.38009889167650357, -10.21368208888610773, 72.75271321436733274 ) ) ;
#23833 = CARTESIAN_POINT ( 'NONE',  ( 44.81606138205700063, 1.441238522345979600, 68.80501292737000085 ) ) ;
#23834 = CARTESIAN_POINT ( 'NONE',  ( 39.95015449827720744, -26.61368208888610809, 70.79240656858104330 ) ) ;
#23835 = VECTOR ( 'NONE', #25270, 1000.000000000000227 ) ;
#23836 = CARTESIAN_POINT ( 'NONE',  ( 40.31606138205700773, -12.76023008545320359, 21.53290024082827969 ) ) ;
#23837 = CARTESIAN_POINT ( 'NONE',  ( 36.87297107704151244, -3.903840866421908196, 70.26145752964255564 ) ) ;
#23838 = PLANE ( 'NONE',  #10438 ) ;
#23839 = VECTOR ( 'NONE', #23692, 1000.000000000000000 ) ;
#23840 = CARTESIAN_POINT ( 'NONE',  ( 38.37017380507018771, -25.60384086642191548, 70.24448340153875847 ) ) ;
#23841 = CARTESIAN_POINT ( 'NONE',  ( 37.69796330110504101, -9.113682088886100985, 69.66206559358663242 ) ) ;
#23842 = CARTESIAN_POINT ( 'NONE',  ( 32.81606138205700773, 34.92314894770293421, 79.37823623207323465 ) ) ;
#23843 = CARTESIAN_POINT ( 'NONE',  ( 39.29254315202757653, -12.80384086642191299, 72.81632618279321889 ) ) ;
#23844 = CARTESIAN_POINT ( 'NONE',  ( 43.81606138205700063, -38.55876147765401640, 70.30501292737012875 ) ) ;
#23845 = CARTESIAN_POINT ( 'NONE',  ( 37.25202387243752611, -9.213682088886100630, 70.00779233799264034 ) ) ;
#23846 = ORIENTED_EDGE ( 'NONE', *, *, #10592, .T. ) ;
#23847 = CARTESIAN_POINT ( 'NONE',  ( 36.07789103942398867, -15.41368208888610347, 70.70992431699450265 ) ) ;
#23848 = ORIENTED_EDGE ( 'NONE', *, *, #21945, .T. ) ;
#23849 = CARTESIAN_POINT ( 'NONE',  ( 31.81606138205700418, 18.19123852234598715, 71.05501292736995822 ) ) ;
#23850 = CARTESIAN_POINT ( 'NONE',  ( 29.64448850680314607, 1.773964314019522925, -3.427682652428152288 ) ) ;
#23851 = CARTESIAN_POINT ( 'NONE',  ( 37.69225076346193504, -17.80384086642191122, 70.42958956619168021 ) ) ;
#23852 = VERTEX_POINT ( 'NONE', #22143 ) ;
#23853 = AXIS2_PLACEMENT_3D ( 'NONE', #14578, #2970, #4919 ) ;
#23854 = VERTEX_POINT ( 'NONE', #6681 ) ;
#23855 = DIRECTION ( 'NONE',  ( -1.156482317317872465E-16, -0.4425581086832399702, 0.8967398287344626739 ) ) ;
#23856 = LINE ( 'NONE', #12422, #6694 ) ;
#23857 = CARTESIAN_POINT ( 'NONE',  ( 37.61123632939164452, -25.70384086642191690, 69.02690120949091579 ) ) ;
#23858 = CIRCLE ( 'NONE', #12780, 4.000000000000000000 ) ;
#23859 = DIRECTION ( 'NONE',  ( -1.000000000000000000, 5.204170427930415223E-30, 1.734723475976805122E-15 ) ) ;
#23860 = CARTESIAN_POINT ( 'NONE',  ( 40.14115730948191185, -26.51368208888610667, 71.32335560751958781 ) ) ;
#23861 = CARTESIAN_POINT ( 'NONE',  ( 38.31606138205699352, 43.35512946304240245, 81.37823623207320622 ) ) ;
#23862 = EDGE_CURVE ( 'NONE', #21235, #4126, #8377, .T. ) ;
#23863 = VERTEX_POINT ( 'NONE', #10435 ) ;
#23864 = CARTESIAN_POINT ( 'NONE',  ( 33.31606138205700773, -22.22127907754186893, 75.80501292736997243 ) ) ;
#23865 = EDGE_CURVE ( 'NONE', #2245, #4112, #8117, .T. ) ;
#23866 = DIRECTION ( 'NONE',  ( -1.000000000000000000, -1.000000000000000078E-15, 0.000000000000000000 ) ) ;
#23867 = CARTESIAN_POINT ( 'NONE',  ( 36.49096545463212493, -20.10384086642191193, 71.32335560751961623 ) ) ;
#23868 = ADVANCED_FACE ( 'NONE', ( #18297 ), #14042, .F. ) ;
#23869 = FILL_AREA_STYLE_COLOUR ( '', #24041 ) ;
#23870 = CARTESIAN_POINT ( 'NONE',  ( 43.31606138205700063, -13.04008168869994222, 21.66778101221729713 ) ) ;
#23871 = EDGE_CURVE ( 'NONE', #22818, #2214, #23050, .T. ) ;
#23872 = EDGE_CURVE ( 'NONE', #9810, #3466, #17123, .T. ) ;
#23873 = ORIENTED_EDGE ( 'NONE', *, *, #18776, .F. ) ;
#23874 = CIRCLE ( 'NONE', #12794, 4.000000000000000000 ) ;
#23875 = CARTESIAN_POINT ( 'NONE',  ( 42.56606138205700063, 3.151453266960317023, 6.397347472316774031 ) ) ;
#23876 = CIRCLE ( 'NONE', #16073, 3.000000000000002665 ) ;
#23877 = DIRECTION ( 'NONE',  ( -1.000000000000000000, 0.000000000000000000, 0.000000000000000000 ) ) ;
#23878 = CARTESIAN_POINT ( 'NONE',  ( 37.21915885897815457, -0.2038408664219102107, 71.67976084211552745 ) ) ;
#23879 = PLANE ( 'NONE',  #18921 ) ;
#23880 = ORIENTED_EDGE ( 'NONE', *, *, #802, .T. ) ;
#23881 = EDGE_CURVE ( 'NONE', #4447, #8708, #17316, .T. ) ;
#23882 = CARTESIAN_POINT ( 'NONE',  ( 39.98359781491296161, -28.41368208888610525, 71.86517103874045631 ) ) ;
#23883 = EDGE_LOOP ( 'NONE', ( #11704, #19120, #5905, #15367 ) ) ;
#23884 = ORIENTED_EDGE ( 'NONE', *, *, #18105, .T. ) ;
#23885 = CARTESIAN_POINT ( 'NONE',  ( 44.81606138205700063, -24.55876147765401996, 67.80501292737008612 ) ) ;
#23886 = EDGE_CURVE ( 'NONE', #24510, #8968, #7326, .T. ) ;
#23887 = DIRECTION ( 'NONE',  ( 0.000000000000000000, 0.000000000000000000, -1.000000000000000000 ) ) ;
#23888 = UNCERTAINTY_MEASURE_WITH_UNIT (LENGTH_MEASURE( 1.000000000000000082E-05 ), #1018, 'distance_accuracy_value', 'NONE');
#23889 = CARTESIAN_POINT ( 'NONE',  ( 38.26194895904383486, -5.013682088886101340, 70.24448340153877268 ) ) ;
#23890 = CARTESIAN_POINT ( 'NONE',  ( 37.12184278917507640, -5.513682088886102228, 71.43714994484035685 ) ) ;
#23891 = VERTEX_POINT ( 'NONE', #16727 ) ;
#23892 = EDGE_LOOP ( 'NONE', ( #8906, #23288, #14257, #18277 ) ) ;
#23893 = CARTESIAN_POINT ( 'NONE',  ( 33.31606138205700773, 3.099306811489555891, 65.29760936252343129 ) ) ;
#23894 = DIRECTION ( 'NONE',  ( 1.000000000000000000, 0.000000000000000000, -0.000000000000000000 ) ) ;
#23895 = ORIENTED_EDGE ( 'NONE', *, *, #22162, .F. ) ;
#23896 = CARTESIAN_POINT ( 'NONE',  ( 32.81606138205700773, 2.761903742731119049, 12.21527246050395377 ) ) ;
#23897 = CARTESIAN_POINT ( 'NONE',  ( 40.14115730948191185, -11.10384086642191015, 71.43714994484034264 ) ) ;
#23898 = DIRECTION ( 'NONE',  ( 0.000000000000000000, -1.000000000000000000, 2.999999999999999839E-15 ) ) ;
#23899 = CARTESIAN_POINT ( 'NONE',  ( 43.81606138205700063, 6.191238522346989903, 65.80501292736998664 ) ) ;
#23900 = ORIENTED_EDGE ( 'NONE', *, *, #19086, .F. ) ;
#23901 = ORIENTED_EDGE ( 'NONE', *, *, #7075, .T. ) ;
#23902 = VECTOR ( 'NONE', #13370, 1000.000000000000000 ) ;
#23903 = EDGE_LOOP ( 'NONE', ( #17544, #13911, #115, #13636 ) ) ;
#23904 = CARTESIAN_POINT ( 'NONE',  ( 33.56606138205700773, 43.19123852234601202, 79.18605660143489899 ) ) ;
#23905 = CARTESIAN_POINT ( 'NONE',  ( 38.82593461698262871, -6.913682088886100807, 69.62690120949091011 ) ) ;
#23906 = DIRECTION ( 'NONE',  ( -1.000000000000000000, 1.115179377413661005E-30, 3.717264591378870232E-16 ) ) ;
#23907 = DIRECTION ( 'NONE',  ( -0.000000000000000000, -3.469446951953613400E-15, -1.000000000000000000 ) ) ;
#23908 = EDGE_CURVE ( 'NONE', #17348, #22306, #15047, .T. ) ;
#23909 = EDGE_CURVE ( 'NONE', #15432, #1244, #10692, .T. ) ;
#23910 = DIRECTION ( 'NONE',  ( 1.000000000000000000, 0.000000000000000000, -0.000000000000000000 ) ) ;
#23911 = CARTESIAN_POINT ( 'NONE',  ( 40.19479760108050215, -29.10876147765365829, 71.16487613871139217 ) ) ;
#23912 = FACE_OUTER_BOUND ( 'NONE', #2836, .T. ) ;
#23913 = DIRECTION ( 'NONE',  ( 0.000000000000000000, -0.5706330172266839140, 0.8212051873014264425 ) ) ;
#23914 = EDGE_LOOP ( 'NONE', ( #3036, #2854, #11809, #21326 ) ) ;
#23915 = DIRECTION ( 'NONE',  ( -2.727049986597863807E-15, 0.7516416929448760387, 0.6595716529892418079 ) ) ;
#23916 = ORIENTED_EDGE ( 'NONE', *, *, #8810, .F. ) ;
#23917 = ORIENTED_EDGE ( 'NONE', *, *, #6981, .T. ) ;
#23918 = LINE ( 'NONE', #12726, #12030 ) ;
#23919 = CARTESIAN_POINT ( 'NONE',  ( 40.33642880535521869, -1.303840866421910105, 69.98269868914867686 ) ) ;
#23920 = ORIENTED_EDGE ( 'NONE', *, *, #24360, .F. ) ;
#23921 = PRESENTATION_LAYER_ASSIGNMENT (  '', '', ( #21879 ) ) ;
#23922 = DIRECTION ( 'NONE',  ( 2.792262043613788535E-15, -0.8967398287344627850, -0.4425581086832399147 ) ) ;
#23923 = CARTESIAN_POINT ( 'NONE',  ( 39.82603832034400426, -10.31368208888610383, 72.40698646996135324 ) ) ;
#23924 = ORIENTED_EDGE ( 'NONE', *, *, #14916, .F. ) ;
#23925 = CARTESIAN_POINT ( 'NONE',  ( 41.31606138205687273, 33.19123852234596939, 65.30501292736991559 ) ) ;
#23926 = EDGE_CURVE ( 'NONE', #20311, #4444, #10309, .T. ) ;
#23927 = CARTESIAN_POINT ( 'NONE',  ( 36.98690846071097837, -17.81368208888610738, 73.30173637941818754 ) ) ;
#23928 = FACE_OUTER_BOUND ( 'NONE', #7008, .T. ) ;
#23929 = DIRECTION ( 'NONE',  ( 1.000000000000000000, 0.000000000000000000, 0.000000000000000000 ) ) ;
#23930 = VECTOR ( 'NONE', #782, 1000.000000000000000 ) ;
#23931 = LINE ( 'NONE', #19829, #6283 ) ;
#23932 = PRESENTATION_STYLE_ASSIGNMENT (( #20209 ) ) ;
#23933 = DIRECTION ( 'NONE',  ( -1.000000000000000000, 0.000000000000000000, 0.000000000000000000 ) ) ;
#23934 = VECTOR ( 'NONE', #6698, 1000.000000000000000 ) ;
#23935 = CARTESIAN_POINT ( 'NONE',  ( 43.06085842172421252, 3.410736059654636332, 6.350806888899277247 ) ) ;
#23936 = CARTESIAN_POINT ( 'NONE',  ( 32.81606138205700773, -36.10876147765401356, 70.30501292737011454 ) ) ;
#23937 = CARTESIAN_POINT ( 'NONE',  ( 39.51027997493896748, -24.51368208888610312, 71.32335560751960202 ) ) ;
#23938 = ORIENTED_EDGE ( 'NONE', *, *, #10359, .T. ) ;
#23939 = CARTESIAN_POINT ( 'NONE',  ( 39.82744760895728575, -21.53744251712932822, 75.32291780635701173 ) ) ;
#23940 = DIRECTION ( 'NONE',  ( 1.000000000000000000, 3.046345864243081498E-15, 1.366653866685770437E-16 ) ) ;
#23941 = EDGE_LOOP ( 'NONE', ( #2343, #23505, #19327, #3798 ) ) ;
#23942 = ORIENTED_EDGE ( 'NONE', *, *, #21225, .F. ) ;
#23943 = UNCERTAINTY_MEASURE_WITH_UNIT (LENGTH_MEASURE( 1.000000000000000082E-05 ), #3543, 'distance_accuracy_value', 'NONE');
#23944 = CARTESIAN_POINT ( 'NONE',  ( 40.26954217208372455, -20.90384086642191974, 72.86986841596734621 ) ) ;
#23945 = CARTESIAN_POINT ( 'NONE',  ( 38.26194895904383486, -29.01368208888610312, 69.64448340153876416 ) ) ;
#23946 = CARTESIAN_POINT ( 'NONE',  ( 44.81606138205700063, -24.55876147765400574, 72.80501292737008612 ) ) ;
#23947 = VECTOR ( 'NONE', #2291, 1000.000000000000000 ) ;
#23948 = ADVANCED_FACE ( 'NONE', ( #13132 ), #5145, .T. ) ;
#23949 = EDGE_CURVE ( 'NONE', #17786, #9852, #18790, .T. ) ;
#23950 = DIRECTION ( 'NONE',  ( 0.000000000000000000, 0.6568589528324746407, -0.7540134720837717852 ) ) ;
#23951 = EDGE_LOOP ( 'NONE', ( #489, #16681 ) ) ;
#23952 = CARTESIAN_POINT ( 'NONE',  ( 39.76340311107733783, -5.792909836048790062, 82.78776523435020351 ) ) ;
#23953 = DIRECTION ( 'NONE',  ( -1.327674326049719602E-15, 0.4425581086832399147, -0.8967398287344627850 ) ) ;
#23954 = VECTOR ( 'NONE', #24803, 1000.000000000000227 ) ;
#23955 = CARTESIAN_POINT ( 'NONE',  ( 37.50301148336529877, -0.5038408664219187205, 73.69843995877330656 ) ) ;
#23956 = CARTESIAN_POINT ( 'NONE',  ( 41.31606138205687273, 42.19123852234599781, 75.30501292736987295 ) ) ;
#23957 = DIRECTION ( 'NONE',  ( -2.417197558325568929E-15, 0.6529557272876933549, 0.7573960774932753104 ) ) ;
#23958 = CARTESIAN_POINT ( 'NONE',  ( 38.37017380507020192, -6.013682088886109334, 73.11602215082118050 ) ) ;
#23959 = CARTESIAN_POINT ( 'NONE',  ( 36.10895460087045450, 8.898345303533549355, 69.30501292736998664 ) ) ;
#23960 = CIRCLE ( 'NONE', #17822, 1.750000000000001554 ) ;
#23961 = CARTESIAN_POINT ( 'NONE',  ( 38.37017380507020192, -26.01368208888611022, 73.11602215082115208 ) ) ;
#23962 = PLANE ( 'NONE',  #19747 ) ;
#23963 = AXIS2_PLACEMENT_3D ( 'NONE', #12975, #14286, #20211 ) ;
#23964 = LINE ( 'NONE', #16721, #24978 ) ;
#23965 = VECTOR ( 'NONE', #6408, 1000.000000000000000 ) ;
#23966 = CARTESIAN_POINT ( 'NONE',  ( 36.31606138205700063, 8.691238522346997897, 68.80501292736998664 ) ) ;
#23967 = CARTESIAN_POINT ( 'NONE',  ( 38.00113996487112189, -25.70384086642191690, 70.22690120949089021 ) ) ;
#23968 = CARTESIAN_POINT ( 'NONE',  ( 37.33957961208646736, -13.81368208888610916, 72.81632618279321889 ) ) ;
#23969 = CARTESIAN_POINT ( 'NONE',  ( 30.81606138205698286, -3.270329303098768126, -7.854091020184564620 ) ) ;
#23970 = VECTOR ( 'NONE', #5188, 1000.000000000000000 ) ;
#23971 = CARTESIAN_POINT ( 'NONE',  ( 37.25202387243754032, -10.40384086642191441, 72.75271321436733274 ) ) ;
#23972 = CARTESIAN_POINT ( 'NONE',  ( 45.81606138205700063, 46.92314894770294131, 81.17823623207318917 ) ) ;
#23973 = CIRCLE ( 'NONE', #16574, 0.7500000000000008882 ) ;
#23974 = CARTESIAN_POINT ( 'NONE',  ( 37.33957961208646736, -13.81368208888610916, 72.81632618279321889 ) ) ;
#23975 = ORIENTED_EDGE ( 'NONE', *, *, #19356, .T. ) ;
#23976 = CARTESIAN_POINT ( 'NONE',  ( 36.11133435605973574, -17.61368208888610454, 72.15350918040385864 ) ) ;
#23977 = ORIENTED_EDGE ( 'NONE', *, *, #7513, .T. ) ;
#23978 = CARTESIAN_POINT ( 'NONE',  ( 43.31606138205700063, -10.66749763588699551, 14.47455635838400134 ) ) ;
#23979 = FACE_BOUND ( 'NONE', #2807, .T. ) ;
#23980 = CARTESIAN_POINT ( 'NONE',  ( 37.31647492878124694, -16.30384086642191122, 72.03616607671141026 ) ) ;
#23981 = VERTEX_POINT ( 'NONE', #1128 ) ;
#23982 = VERTEX_POINT ( 'NONE', #867 ) ;
#23983 = LINE ( 'NONE', #14583, #17908 ) ;
#23984 = FACE_OUTER_BOUND ( 'NONE', #20955, .T. ) ;
#23985 = CARTESIAN_POINT ( 'NONE',  ( 40.77203464402485622, -23.10384086642191548, 71.43714994484032843 ) ) ;
#23986 = AXIS2_PLACEMENT_3D ( 'NONE', #21921, #5829, #5961 ) ;
#23987 = CARTESIAN_POINT ( 'NONE',  ( 43.31606138205700063, -25.26124097814961544, 70.06813202641110649 ) ) ;
#23988 = CARTESIAN_POINT ( 'NONE',  ( 36.87297107704152666, -27.71368208888610241, 72.49904802271738902 ) ) ;
#23989 = PLANE ( 'NONE',  #13497 ) ;
#23990 = EDGE_LOOP ( 'NONE', ( #14620, #20879, #14460, #19398 ) ) ;
#23991 = EDGE_LOOP ( 'NONE', ( #5278, #9837, #17990, #20346 ) ) ;
#23992 = CARTESIAN_POINT ( 'NONE',  ( 33.57054579126889138, 3.412273012123823168, 6.349712035633038987 ) ) ;
#23993 = DIRECTION ( 'NONE',  ( 1.000000000000000000, 2.999999999999999839E-15, 0.000000000000000000 ) ) ;
#23994 = AXIS2_PLACEMENT_3D ( 'NONE', #171, #416, #5987 ) ;
#23995 = EDGE_CURVE ( 'NONE', #17824, #2309, #24696, .T. ) ;
#23996 = CARTESIAN_POINT ( 'NONE',  ( 37.69796330110505522, -20.50384086642191050, 73.09843995877329803 ) ) ;
#23997 = DIRECTION ( 'NONE',  ( 0.000000000000000000, 1.000000000000000000, -6.938893903907402716E-15 ) ) ;
#23998 =( GEOMETRIC_REPRESENTATION_CONTEXT ( 3 ) GLOBAL_UNCERTAINTY_ASSIGNED_CONTEXT ( ( #19055 ) ) GLOBAL_UNIT_ASSIGNED_CONTEXT ( ( #13232, #3295, #23121 ) ) REPRESENTATION_CONTEXT ( 'NONE', 'WORKASPACE' ) );
#23999 = FACE_OUTER_BOUND ( 'NONE', #22245, .T. ) ;
#24000 = LINE ( 'NONE', #9991, #22217 ) ;
#24001 = CARTESIAN_POINT ( 'NONE',  ( 38.00113996487112189, -1.703840866421911571, 70.22690120949091863 ) ) ;
#24002 = CARTESIAN_POINT ( 'NONE',  ( 33.56606138205700773, 42.19123852234601202, 79.18605660143489899 ) ) ;
#24003 = EDGE_LOOP ( 'NONE', ( #6600, #15796, #7578, #20552 ) ) ;
#24004 =( GEOMETRIC_REPRESENTATION_CONTEXT ( 3 ) GLOBAL_UNCERTAINTY_ASSIGNED_CONTEXT ( ( #2499 ) ) GLOBAL_UNIT_ASSIGNED_CONTEXT ( ( #2755, #6638, #20306 ) ) REPRESENTATION_CONTEXT ( 'NONE', 'WORKASPACE' ) );
#24005 = CARTESIAN_POINT ( 'NONE',  ( 45.81606138205696510, -29.47337283097071037, 44.07055847651734837 ) ) ;
#24006 = EDGE_LOOP ( 'NONE', ( #19332, #19777, #25014, #18620 ) ) ;
#24007 = ORIENTED_EDGE ( 'NONE', *, *, #20361, .F. ) ;
#24008 = CARTESIAN_POINT ( 'NONE',  ( 35.31606138205700773, 14.21032488318011211, 61.14033482768515881 ) ) ;
#24009 = CARTESIAN_POINT ( 'NONE',  ( 36.06606138205700063, 2.740850673309605412, 6.112030963703427133 ) ) ;
#24010 = CARTESIAN_POINT ( 'NONE',  ( 37.25260217561390874, -3.613682088886100097, 71.78268878715394408 ) ) ;
#24011 = EDGE_CURVE ( 'NONE', #24485, #21068, #22525, .T. ) ;
#24012 = EDGE_CURVE ( 'NONE', #17666, #11586, #3193, .T. ) ;
#24013 = CARTESIAN_POINT ( 'NONE',  ( 39.31564783533280405, -4.313682088886102051, 72.03616607671141026 ) ) ;
#24014 = EDGE_LOOP ( 'NONE', ( #16677, #16030, #6236, #22031 ) ) ;
#24015 = ORIENTED_EDGE ( 'NONE', *, *, #20096, .F. ) ;
#24016 = CARTESIAN_POINT ( 'NONE',  ( 31.56606138205707168, -38.42645682328038248, 63.90656833300437256 ) ) ;
#24017 = DIRECTION ( 'NONE',  ( 1.000000000000000000, 0.000000000000000000, 0.000000000000000000 ) ) ;
#24018 = ORIENTED_EDGE ( 'NONE', *, *, #20550, .T. ) ;
#24019 = CARTESIAN_POINT ( 'NONE',  ( 43.81606138205700063, 22.19123852234699967, 69.30501292736994401 ) ) ;
#24020 = CARTESIAN_POINT ( 'NONE',  ( 39.82603832034400426, -11.30384086642190944, 70.35351908239857721 ) ) ;
#24021 = EDGE_CURVE ( 'NONE', #23154, #18450, #21830, .T. ) ;
#24022 = DIRECTION ( 'NONE',  ( 1.000000000000000000, 1.246695722929252133E-30, -1.734723475976824844E-16 ) ) ;
#24023 =( GEOMETRIC_REPRESENTATION_CONTEXT ( 3 ) GLOBAL_UNCERTAINTY_ASSIGNED_CONTEXT ( ( #3069 ) ) GLOBAL_UNIT_ASSIGNED_CONTEXT ( ( #19515, #23365, #13465 ) ) REPRESENTATION_CONTEXT ( 'NONE', 'WORKASPACE' ) );
#24024 = CARTESIAN_POINT ( 'NONE',  ( 36.99021717747880444, -21.74946196664538078, 75.82133169473785017 ) ) ;
#24025 = CARTESIAN_POINT ( 'NONE',  ( 45.61606138205700489, 46.92314894770294131, 81.17823623207318917 ) ) ;
#24026 = VERTEX_POINT ( 'NONE', #13004 ) ;
#24027 = AXIS2_PLACEMENT_3D ( 'NONE', #1578, #24511, #16936 ) ;
#24028 = VECTOR ( 'NONE', #12842, 1000.000000000000000 ) ;
#24029 = ORIENTED_EDGE ( 'NONE', *, *, #16846, .T. ) ;
#24030 = ORIENTED_EDGE ( 'NONE', *, *, #12854, .T. ) ;
#24031 = LINE ( 'NONE', #23904, #108 ) ;
#24032 = CARTESIAN_POINT ( 'NONE',  ( 39.95015449827720744, -10.61368208888610631, 70.79240656858107172 ) ) ;
#24033 = AXIS2_PLACEMENT_3D ( 'NONE', #6736, #19889, #12295 ) ;
#24034 = ADVANCED_FACE ( 'NONE', ( #20853 ), #1396, .F. ) ;
#24035 = CARTESIAN_POINT ( 'NONE',  ( 30.81606138205707168, -37.70325315460881654, 65.37863370302704880 ) ) ;
#24036 = FACE_OUTER_BOUND ( 'NONE', #11307, .T. ) ;
#24037 = LINE ( 'NONE', #18136, #11092 ) ;
#24038 = CARTESIAN_POINT ( 'NONE',  ( 39.66066260159681889, -29.10876147764981781, 69.85357445396793707 ) ) ;
#24039 = LINE ( 'NONE', #2652, #13562 ) ;
#24040 = CARTESIAN_POINT ( 'NONE',  ( 44.81606138205700063, -34.55876147765400930, 73.30501292737011454 ) ) ;
#24041 = COLOUR_RGB ( '', 0.72549020, 0.75294118, 0.79215686) ;
#24042 = CARTESIAN_POINT ( 'NONE',  ( 37.42666033486774069, -22.01378883779070961, 75.30711745748108399 ) ) ;
#24043 = EDGE_LOOP ( 'NONE', ( #24072, #5172, #9257, #24383 ) ) ;
#24044 = ORIENTED_EDGE ( 'NONE', *, *, #20472, .T. ) ;
#24045 = DIRECTION ( 'NONE',  ( 0.000000000000000000, -0.5706330172266919076, 0.8212051873014208914 ) ) ;
#24046 = CARTESIAN_POINT ( 'NONE',  ( 40.26954217208372455, -2.903840866421918410, 72.86986841596736042 ) ) ;
#24047 = ADVANCED_FACE ( 'NONE', ( #16993 ), #24826, .T. ) ;
#24048 = EDGE_CURVE ( 'NONE', #8869, #21859, #6193, .T. ) ;
#24049 = ORIENTED_EDGE ( 'NONE', *, *, #20435, .F. ) ;
#24050 = LINE ( 'NONE', #14526, #12436 ) ;
#24051 = CARTESIAN_POINT ( 'NONE',  ( 38.37017380507020192, -8.013682088886108446, 73.11602215082118050 ) ) ;
#24052 = EDGE_CURVE ( 'NONE', #9423, #4892, #16489, .T. ) ;
#24053 = ADVANCED_FACE ( 'NONE', ( #11202 ), #9526, .F. ) ;
#24054 = EDGE_CURVE ( 'NONE', #17582, #21203, #7841, .T. ) ;
#24055 = LINE ( 'NONE', #4364, #18227 ) ;
#24056 = CARTESIAN_POINT ( 'NONE',  ( 40.77203464402485622, -14.51368208888610312, 71.32335560751960202 ) ) ;
#24057 = LINE ( 'NONE', #4494, #9053 ) ;
#24058 = DIRECTION ( 'NONE',  ( 1.000000000000000000, -0.000000000000000000, 0.000000000000000000 ) ) ;
#24059 = EDGE_CURVE ( 'NONE', #5938, #10765, #17244, .T. ) ;
#24060 = EDGE_CURVE ( 'NONE', #17954, #14226, #20184, .T. ) ;
#24061 = DIRECTION ( 'NONE',  ( -5.047295537021760406E-31, 1.000000000000000000, -3.491481338843135327E-15 ) ) ;
#24062 =( NAMED_UNIT ( * ) PLANE_ANGLE_UNIT ( ) SI_UNIT ( $, .RADIAN. ) );
#24063 = CARTESIAN_POINT ( 'NONE',  ( 45.06606138205697221, -4.349482454670840603, -5.142398479549302515 ) ) ;
#24064 = DIRECTION ( 'NONE',  ( 0.000000000000000000, 0.000000000000000000, 1.000000000000000000 ) ) ;
#24065 = CARTESIAN_POINT ( 'NONE',  ( 35.31606138205687273, 33.19123852234595518, 61.30501292736990848 ) ) ;
#24066 = CARTESIAN_POINT ( 'NONE',  ( 37.25260217561390874, -25.61368208888610098, 71.78268878715390144 ) ) ;
#24067 = VERTEX_POINT ( 'NONE', #23282 ) ;
#24068 = DIRECTION ( 'NONE',  ( -1.000000000000000000, 0.000000000000000000, 0.000000000000000000 ) ) ;
#24069 = EDGE_CURVE ( 'NONE', #18865, #20940, #13260, .T. ) ;
#24070 = LINE ( 'NONE', #17920, #18932 ) ;
#24071 = ORIENTED_EDGE ( 'NONE', *, *, #11134, .T. ) ;
#24072 = ORIENTED_EDGE ( 'NONE', *, *, #3910, .F. ) ;
#24073 = CARTESIAN_POINT ( 'NONE',  ( 38.26194895904384197, -20.60384086642191903, 73.71602215082113219 ) ) ;
#24074 = CARTESIAN_POINT ( 'NONE',  ( 36.29569395875879678, 0.6863179111138985045, 69.98269868914869107 ) ) ;
#24075 = DIRECTION ( 'NONE',  ( -1.000000000000000000, -2.999999999999999839E-15, 0.000000000000000000 ) ) ;
#24076 = DIRECTION ( 'NONE',  ( 0.000000000000000000, -0.6568589528324746407, 0.7540134720837716742 ) ) ;
#24077 = ORIENTED_EDGE ( 'NONE', *, *, #1820, .T. ) ;
#24078 = FACE_OUTER_BOUND ( 'NONE', #14107, .T. ) ;
#24079 = DIRECTION ( 'NONE',  ( 0.000000000000000000, -1.000000000000000000, 3.491481338843135327E-15 ) ) ;
#24080 = CARTESIAN_POINT ( 'NONE',  ( 37.50301148336529877, -6.503840866421916722, 73.69843995877330656 ) ) ;
#24081 = PLANE ( 'NONE',  #25064 ) ;
#24082 = FACE_OUTER_BOUND ( 'NONE', #1983, .T. ) ;
#24083 = CARTESIAN_POINT ( 'NONE',  ( 36.68196826583682935, -7.613682088886103649, 71.96809898377890136 ) ) ;
#24084 = DIRECTION ( 'NONE',  ( -1.000000000000000000, 0.000000000000000000, 0.000000000000000000 ) ) ;
#24085 = DIRECTION ( 'NONE',  ( 0.000000000000000000, -1.000000000000000000, 2.999999999999999839E-15 ) ) ;
#24086 = DIRECTION ( 'NONE',  ( -3.154042683594193641E-15, 0.000000000000000000, 1.000000000000000000 ) ) ;
#24087 = EDGE_CURVE ( 'NONE', #2531, #7462, #11716, .T. ) ;
#24088 = FACE_OUTER_BOUND ( 'NONE', #22239, .T. ) ;
#24089 = CARTESIAN_POINT ( 'NONE',  ( 39.24876120206129571, -24.90384086642191264, 72.12822762946746025 ) ) ;
#24090 = CARTESIAN_POINT ( 'NONE',  ( 39.38009889167650357, -12.21368208888610596, 72.75271321436731853 ) ) ;
#24091 = EDGE_CURVE ( 'NONE', #22, #8257, #23858, .T. ) ;
#24092 = DIRECTION ( 'NONE',  ( 1.000000000000000000, 0.000000000000000000, 0.000000000000000000 ) ) ;
#24093 = CARTESIAN_POINT ( 'NONE',  ( 38.82593461698265003, -10.70384086642191690, 73.13360434286904876 ) ) ;
#24094 = CARTESIAN_POINT ( 'NONE',  ( 44.81606138205700063, -34.55876147765400930, 73.30501292737011454 ) ) ;
#24095 =( REPRESENTATION_RELATIONSHIP ('NONE','NONE', #17377, #10266 ) REPRESENTATION_RELATIONSHIP_WITH_TRANSFORMATION ( #18188 )SHAPE_REPRESENTATION_RELATIONSHIP( ) );
#24096 = CARTESIAN_POINT ( 'NONE',  ( 38.93415946300897446, -12.11368208888610276, 73.09843995877329803 ) ) ;
#24097 = ORIENTED_EDGE ( 'NONE', *, *, #22166, .T. ) ;
#24098 = CARTESIAN_POINT ( 'NONE',  ( 36.89935272106204422, -13.21368208888610241, 69.52238214136768590 ) ) ;
#24099 = ORIENTED_EDGE ( 'NONE', *, *, #8278, .T. ) ;
#24100 = LINE ( 'NONE', #22183, #19749 ) ;
#24101 = CARTESIAN_POINT ( 'NONE',  ( 43.81606138205700063, -34.55876147765403061, 66.30501292737011454 ) ) ;
#24102 = CARTESIAN_POINT ( 'NONE',  ( 37.21915885897815457, -20.20384086642191335, 71.67976084211552745 ) ) ;
#24103 = VERTEX_POINT ( 'NONE', #1631 ) ;
#24104 = ORIENTED_EDGE ( 'NONE', *, *, #23926, .F. ) ;
#24105 = DIRECTION ( 'NONE',  ( 0.000000000000000000, 1.000000000000000000, 0.000000000000000000 ) ) ;
#24106 = CARTESIAN_POINT ( 'NONE',  ( 45.81606138205697221, -3.270329303098730822, -7.854091020184544192 ) ) ;
#24107 = CARTESIAN_POINT ( 'NONE',  ( 36.07789103942399578, -22.20384086642191690, 72.05058123536544201 ) ) ;
#24108 = CARTESIAN_POINT ( 'NONE',  ( 33.31606138205700773, 4.124002793203064066, 6.312068993173404863 ) ) ;
#24109 = CARTESIAN_POINT ( 'NONE',  ( 40.14115730948191185, -24.51368208888609601, 71.32335560751958781 ) ) ;
#24110 = DIRECTION ( 'NONE',  ( 0.000000000000000000, -1.000000000000000000, 2.999999999999999839E-15 ) ) ;
#24111 = ORIENTED_EDGE ( 'NONE', *, *, #19311, .T. ) ;
#24112 = DIRECTION ( 'NONE',  ( -0.000000000000000000, -3.469446951953613400E-15, -1.000000000000000000 ) ) ;
#24113 = DIRECTION ( 'NONE',  ( 1.000000000000000000, 3.091505625455829092E-15, 4.515976121274730398E-17 ) ) ;
#24114 = CARTESIAN_POINT ( 'NONE',  ( 39.95015449827720744, -13.00384086642191228, 71.96809898377887293 ) ) ;
#24115 = ADVANCED_FACE ( 'NONE', ( #15433 ), #19679, .F. ) ;
#24116 = FACE_OUTER_BOUND ( 'NONE', #15962, .T. ) ;
#24117 = EDGE_CURVE ( 'NONE', #17790, #6859, #25068, .T. ) ;
#24118 = EDGE_LOOP ( 'NONE', ( #1372, #21060, #13041, #682, #12247, #21090, #22058, #9248, #12109 ) ) ;
#24119 = DIRECTION ( 'NONE',  ( 0.000000000000000000, 1.000000000000000000, 0.000000000000000000 ) ) ;
#24120 = CARTESIAN_POINT ( 'NONE',  ( 44.81606138205700063, -24.55876147765401996, 67.80501292737008612 ) ) ;
#24121 = CARTESIAN_POINT ( 'NONE',  ( 39.02742774030101458, -1.403840866421909972, 70.49320253461759478 ) ) ;
#24122 = LINE ( 'NONE', #431, #14793 ) ;
#24123 = ORIENTED_EDGE ( 'NONE', *, *, #13505, .F. ) ;
#24124 = FACE_BOUND ( 'NONE', #9908, .T. ) ;
#24125 = ORIENTED_EDGE ( 'NONE', *, *, #18080, .F. ) ;
#24126 = ORIENTED_EDGE ( 'NONE', *, *, #4207, .T. ) ;
#24127 = DIRECTION ( 'NONE',  ( -1.000000000000000000, 0.000000000000000000, 0.000000000000000000 ) ) ;
#24128 = DIRECTION ( 'NONE',  ( 0.000000000000000000, -1.000000000000000000, 2.999999999999999839E-15 ) ) ;
#24129 = UNCERTAINTY_MEASURE_WITH_UNIT (LENGTH_MEASURE( 1.000000000000000082E-05 ), #12385, 'distance_accuracy_value', 'NONE');
#24130 = CARTESIAN_POINT ( 'NONE',  ( 38.93987200065208754, -4.813682088886099386, 70.42958956619168021 ) ) ;
#24131 = CARTESIAN_POINT ( 'NONE',  ( 37.25260217561390874, -5.613682088886101873, 71.78268878715394408 ) ) ;
#24132 = ORIENTED_EDGE ( 'NONE', *, *, #21669, .T. ) ;
#24133 = ORIENTED_EDGE ( 'NONE', *, *, #491, .F. ) ;
#24134 = DIRECTION ( 'NONE',  ( -1.000000000000000000, 0.000000000000000000, 0.000000000000000000 ) ) ;
#24135 = EDGE_CURVE ( 'NONE', #10246, #20035, #23404, .T. ) ;
#24136 = CARTESIAN_POINT ( 'NONE',  ( 43.31606138205700063, -12.40281258615395465, 20.95421293576468358 ) ) ;
#24137 = ORIENTED_EDGE ( 'NONE', *, *, #5400, .F. ) ;
#24138 = DIRECTION ( 'NONE',  ( 1.000000000000000000, 0.000000000000000000, 0.000000000000000000 ) ) ;
#24139 = CARTESIAN_POINT ( 'NONE',  ( 39.82603832034400426, -9.303840866421907663, 70.35351908239857721 ) ) ;
#24140 = VECTOR ( 'NONE', #18876, 1000.000000000000000 ) ;
#24141 = VECTOR ( 'NONE', #12265, 1000.000000000000000 ) ;
#24142 = VECTOR ( 'NONE', #16029, 1000.000000000000227 ) ;
#24143 = CARTESIAN_POINT ( 'NONE',  ( 36.31606138205702194, -20.02093502212016318, 26.61211107664843212 ) ) ;
#24144 = LINE ( 'NONE', #10519, #6465 ) ;
#24145 = ORIENTED_EDGE ( 'NONE', *, *, #6414, .F. ) ;
#24146 = ORIENTED_EDGE ( 'NONE', *, *, #5779, .F. ) ;
#24147 = VERTEX_POINT ( 'NONE', #11334 ) ;
#24148 = CARTESIAN_POINT ( 'NONE',  ( 43.31606138205700063, -10.80800258567212602, 32.62011605800211811 ) ) ;
#24149 = CARTESIAN_POINT ( 'NONE',  ( 37.33957961208646736, -5.813682088886107380, 72.81632618279323310 ) ) ;
#24150 = DIRECTION ( 'NONE',  ( 1.000000000000000000, -0.000000000000000000, 0.000000000000000000 ) ) ;
#24151 = CARTESIAN_POINT ( 'NONE',  ( 44.81606138205700063, 41.44123852234595518, 61.30501292736988006 ) ) ;
#24152 = AXIS2_PLACEMENT_3D ( 'NONE', #22691, #9061, #4672 ) ;
#24153 = PLANE ( 'NONE',  #24641 ) ;
#24154 = DIRECTION ( 'NONE',  ( 1.734723475976805122E-15, 2.999999999999999839E-15, 1.000000000000000000 ) ) ;
#24155 = AXIS2_PLACEMENT_3D ( 'NONE', #15980, #8024, #24086 ) ;
#24156 = VECTOR ( 'NONE', #15657, 1000.000000000000000 ) ;
#24157 = DIRECTION ( 'NONE',  ( -1.000000000000000000, -1.734723475976804876E-16, 1.734723475976814737E-16 ) ) ;
#24158 = ORIENTED_EDGE ( 'NONE', *, *, #24011, .F. ) ;
#24159 = VERTEX_POINT ( 'NONE', #17371 ) ;
#24160 = LINE ( 'NONE', #601, #2951 ) ;
#24161 = CARTESIAN_POINT ( 'NONE',  ( 36.11133435605973574, -27.61368208888610809, 72.15350918040381600 ) ) ;
#24162 = CARTESIAN_POINT ( 'NONE',  ( 37.60469502381300089, -21.21368208888610241, 70.49320253461759478 ) ) ;
#24163 = ORIENTED_EDGE ( 'NONE', *, *, #9884, .T. ) ;
#24164 = ORIENTED_EDGE ( 'NONE', *, *, #20884, .T. ) ;
#24165 = CARTESIAN_POINT ( 'NONE',  ( 29.81606138205707879, -38.42645682328038959, 63.90656833300437256 ) ) ;
#24166 = CARTESIAN_POINT ( 'NONE',  ( 36.64852494920107517, -5.413682088886106136, 70.89533451361948835 ) ) ;
#24167 = CARTESIAN_POINT ( 'NONE',  ( 37.25202387243754032, -28.40384086642191619, 72.75271321436730432 ) ) ;
#24168 = DIRECTION ( 'NONE',  ( 0.000000000000000000, 0.5706330172266920187, -0.8212051873014210024 ) ) ;
#24169 = CARTESIAN_POINT ( 'NONE',  ( 40.52078840805428683, -6.613682088886105426, 70.60699637195608602 ) ) ;
#24170 = VECTOR ( 'NONE', #14804, 1000.000000000000114 ) ;
#24171 = DIRECTION ( 'NONE',  ( 1.000000000000000000, 0.000000000000000000, 0.000000000000000000 ) ) ;
#24172 = VECTOR ( 'NONE', #6781, 1000.000000000000000 ) ;
#24173 = LINE ( 'NONE', #12496, #10809 ) ;
#24174 = CARTESIAN_POINT ( 'NONE',  ( 44.31606138205700063, 10.62769494289597993, 68.29765714199933768 ) ) ;
#24175 = LINE ( 'NONE', #2419, #20245 ) ;
#24176 = EDGE_CURVE ( 'NONE', #10990, #5522, #19770, .T. ) ;
#24177 = EDGE_CURVE ( 'NONE', #12724, #15674, #13389, .T. ) ;
#24178 = CARTESIAN_POINT ( 'NONE',  ( 43.52392165233022325, 3.236692751922551459, 6.150480132932879762 ) ) ;
#24179 = EDGE_CURVE ( 'NONE', #14019, #16125, #13765, .T. ) ;
#24180 = EDGE_CURVE ( 'NONE', #4087, #6765, #4543, .T. ) ;
#24181 = FACE_OUTER_BOUND ( 'NONE', #7948, .T. ) ;
#24182 = EDGE_CURVE ( 'NONE', #21730, #2758, #17757, .T. ) ;
#24183 = EDGE_LOOP ( 'NONE', ( #4507, #6440, #14610, #9492 ) ) ;
#24184 = CARTESIAN_POINT ( 'NONE',  ( 38.58006293444520196, -22.20809853857948823, 75.29993851755294543 ) ) ;
#24185 = DIRECTION ( 'NONE',  ( 1.000000000000000000, 2.440719103442460911E-15, 1.328886038262200866E-15 ) ) ;
#24186 = ORIENTED_EDGE ( 'NONE', *, *, #22532, .F. ) ;
#24187 = ORIENTED_EDGE ( 'NONE', *, *, #17022, .T. ) ;
#24188 = UNCERTAINTY_MEASURE_WITH_UNIT (LENGTH_MEASURE( 1.000000000000000082E-05 ), #11078, 'distance_accuracy_value', 'NONE');
#24189 = CARTESIAN_POINT ( 'NONE',  ( 39.02088643472237806, -22.70384086642191690, 73.73360434286898624 ) ) ;
#24190 = VECTOR ( 'NONE', #2018, 1000.000000000000000 ) ;
#24191 = CARTESIAN_POINT ( 'NONE',  ( 39.38009889167650357, -28.21368208888610951, 72.75271321436730432 ) ) ;
#24192 = CARTESIAN_POINT ( 'NONE',  ( 34.06606138205689405, 3.151453266960317023, 6.397347472316774031 ) ) ;
#24193 = EDGE_CURVE ( 'NONE', #21091, #21783, #9656, .T. ) ;
#24194 = FACE_OUTER_BOUND ( 'NONE', #25286, .T. ) ;
#24195 = CARTESIAN_POINT ( 'NONE',  ( 39.59324923284151510, -28.74115096347518161, 70.20355626897213597 ) ) ;
#24196 = ORIENTED_EDGE ( 'NONE', *, *, #21284, .T. ) ;
#24197 = DIRECTION ( 'NONE',  ( 1.000000000000000000, -5.510910596163088391E-31, -1.836970198721029688E-16 ) ) ;
#24198 = CARTESIAN_POINT ( 'NONE',  ( 31.56606138205697576, -4.349482454670882348, -5.142398479549302515 ) ) ;
#24199 = CARTESIAN_POINT ( 'NONE',  ( 40.33642880535521869, -1.303840866421910105, 69.98269868914867686 ) ) ;
#24200 = DIRECTION ( 'NONE',  ( 0.000000000000000000, 0.7540134720837725624, 0.6568589528324736415 ) ) ;
#24201 = CARTESIAN_POINT ( 'NONE',  ( 36.80608444377001121, -9.313682088886100274, 70.35351908239860563 ) ) ;
#24202 = DIRECTION ( 'NONE',  ( 0.000000000000000000, 1.000000000000000000, 0.000000000000000000 ) ) ;
#24203 = EDGE_CURVE ( 'NONE', #1142, #8061, #17507, .T. ) ;
#24204 = CARTESIAN_POINT ( 'NONE',  ( 39.95015449827720744, -18.61368208888610454, 70.79240656858105751 ) ) ;
#24205 = VECTOR ( 'NONE', #19113, 1000.000000000000000 ) ;
#24206 = DIRECTION ( 'NONE',  ( 3.771137991253929559E-16, -0.8212051873014208914, -0.5706330172266919076 ) ) ;
#24207 = DIRECTION ( 'NONE',  ( -1.933202721249430383E-16, 0.9925461516413217611, -0.1218693434051499741 ) ) ;
#24208 = AXIS2_PLACEMENT_3D ( 'NONE', #7993, #6432, #22136 ) ;
#24209 = CARTESIAN_POINT ( 'NONE',  ( 37.89291511884479036, -26.50384086642191406, 72.49843995877328950 ) ) ;
#24210 = CARTESIAN_POINT ( 'NONE',  ( 39.98359781491296161, -14.41368208888610525, 71.86517103874047052 ) ) ;
#24211 = VERTEX_POINT ( 'NONE', #2024 ) ;
#24212 = PLANE ( 'NONE',  #13151 ) ;
#24213 = VERTEX_POINT ( 'NONE', #3834 ) ;
#24214 = VECTOR ( 'NONE', #22898, 1000.000000000000000 ) ;
#24215 = CARTESIAN_POINT ( 'NONE',  ( 38.26194895904384907, -14.60384086642191548, 73.11602215082116629 ) ) ;
#24216 = CARTESIAN_POINT ( 'NONE',  ( 41.81606138205696510, -1.316127829577467656, -4.808842309729777220 ) ) ;
#24217 = CARTESIAN_POINT ( 'NONE',  ( 37.69796330110504101, -3.113682088886098764, 69.66206559358663242 ) ) ;
#24218 = ORIENTED_EDGE ( 'NONE', *, *, #5989, .F. ) ;
#24219 = CARTESIAN_POINT ( 'NONE',  ( 37.50301148336529167, -13.11368208888610454, 69.06206559358665231 ) ) ;
#24220 = ORIENTED_EDGE ( 'NONE', *, *, #18399, .T. ) ;
#24221 = DIRECTION ( 'NONE',  ( 0.000000000000000000, -1.000000000000000000, 3.129456975819164530E-15 ) ) ;
#24222 = CARTESIAN_POINT ( 'NONE',  ( 31.91606138205697718, -5.022037326221728826, -5.474317061061731771 ) ) ;
#24223 = CARTESIAN_POINT ( 'NONE',  ( 37.21915885897815457, -12.20384086642191157, 71.67976084211552745 ) ) ;
#24224 = VECTOR ( 'NONE', #24092, 1000.000000000000000 ) ;
#24225 = ORIENTED_EDGE ( 'NONE', *, *, #20519, .F. ) ;
#24226 = VERTEX_POINT ( 'NONE', #9775 ) ;
#24227 = CARTESIAN_POINT ( 'NONE',  ( 45.81606138205700063, -34.55876147765410167, 70.30501292737000085 ) ) ;
#24228 = CARTESIAN_POINT ( 'NONE',  ( 45.81606138205700063, -36.05876147765410877, 70.30501292737000085 ) ) ;
#24229 = CARTESIAN_POINT ( 'NONE',  ( 38.26194895904384197, -20.60384086642191903, 73.71602215082113219 ) ) ;
#24230 = DIRECTION ( 'NONE',  ( 0.000000000000000000, -1.000000000000000000, 6.938893903907222067E-15 ) ) ;
#24231 = CARTESIAN_POINT ( 'NONE',  ( 39.95015449827720744, -24.61368208888610454, 70.79240656858104330 ) ) ;
#24232 = FACE_OUTER_BOUND ( 'NONE', #9550, .T. ) ;
#24233 = EDGE_CURVE ( 'NONE', #14953, #536, #25461, .T. ) ;
#24234 = DIRECTION ( 'NONE',  ( 0.000000000000000000, 1.000000000000000000, -5.551115123125785858E-15 ) ) ;
#24235 = EDGE_CURVE ( 'NONE', #13201, #22354, #4605, .T. ) ;
#24236 = AXIS2_PLACEMENT_3D ( 'NONE', #19677, #20188, #23671 ) ;
#24237 = ORIENTED_EDGE ( 'NONE', *, *, #10067, .T. ) ;
#24238 = FACE_OUTER_BOUND ( 'NONE', #18792, .T. ) ;
#24239 = DIRECTION ( 'NONE',  ( 0.000000000000000000, 2.999999999999999839E-15, 1.000000000000000000 ) ) ;
#24240 = VECTOR ( 'NONE', #1935, 1000.000000000000000 ) ;
#24241 = CARTESIAN_POINT ( 'NONE',  ( 38.82593461698264292, -16.70384086642191690, 73.13360434286903455 ) ) ;
#24242 = PRODUCT_CONTEXT ( 'NONE', #24918, 'mechanical' ) ;
#24243 = DIRECTION ( 'NONE',  ( 1.000000000000000000, 1.734723475976804876E-16, -1.734723475976814737E-16 ) ) ;
#24244 = CIRCLE ( 'NONE', #5353, 0.7500000000000006661 ) ;
#24245 = EDGE_LOOP ( 'NONE', ( #13531, #11304, #20676, #8600 ) ) ;
#24246 = CARTESIAN_POINT ( 'NONE',  ( 33.31606138205700773, -10.80800258567212602, 32.62011605800211811 ) ) ;
#24247 = FACE_OUTER_BOUND ( 'NONE', #4606, .T. ) ;
#24248 = CARTESIAN_POINT ( 'NONE',  ( 38.26194895904384907, -28.60384086642191548, 73.11602215082115208 ) ) ;
#24249 = VECTOR ( 'NONE', #8658, 1000.000000000000000 ) ;
#24250 = CARTESIAN_POINT ( 'NONE',  ( 37.79523030992096011, -5.265654987800329145, 82.79985390080808827 ) ) ;
#24251 = VERTEX_POINT ( 'NONE', #18016 ) ;
#24252 = AXIS2_PLACEMENT_3D ( 'NONE', #11903, #15370, #5587 ) ;
#24253 = CARTESIAN_POINT ( 'NONE',  ( 38.37017380507020192, -24.01368208888610667, 73.11602215082115208 ) ) ;
#24254 = ORIENTED_EDGE ( 'NONE', *, *, #9912, .T. ) ;
#24255 = EDGE_LOOP ( 'NONE', ( #12592, #4469, #3993, #10538 ) ) ;
#24256 = DIRECTION ( 'NONE',  ( -1.000000000000000000, -2.999999999999999839E-15, 0.000000000000000000 ) ) ;
#24257 = CARTESIAN_POINT ( 'NONE',  ( 31.81606138205700418, 18.19123852234599070, 72.05501292736995822 ) ) ;
#24258 = VECTOR ( 'NONE', #16091, 1000.000000000000000 ) ;
#24259 = CARTESIAN_POINT ( 'NONE',  ( 39.41296390513587511, -8.413682088886101695, 71.67976084211552745 ) ) ;
#24260 = CARTESIAN_POINT ( 'NONE',  ( 38.26194895904383486, -5.013682088886101340, 70.24448340153877268 ) ) ;
#24261 = ORIENTED_EDGE ( 'NONE', *, *, #16102, .T. ) ;
#24262 = ORIENTED_EDGE ( 'NONE', *, *, #16831, .F. ) ;
#24263 = CARTESIAN_POINT ( 'NONE',  ( 38.31606138205699352, 42.82479937715250173, 82.59790614618330551 ) ) ;
#24264 = DIRECTION ( 'NONE',  ( -1.000000000000000000, 1.040834085586084551E-30, 3.469446951953615175E-16 ) ) ;
#24265 = ORIENTED_EDGE ( 'NONE', *, *, #1627, .F. ) ;
#24266 = CARTESIAN_POINT ( 'NONE',  ( 43.31606138205700063, -13.25716901376041967, 21.21736665487721041 ) ) ;
#24267 = CARTESIAN_POINT ( 'NONE',  ( 39.98359781491296161, -9.203840866421911571, 70.89533451361947414 ) ) ;
#24268 = ADVANCED_FACE ( 'NONE', ( #6287 ), #16438, .T. ) ;
#24269 = ADVANCED_BREP_SHAPE_REPRESENTATION ( '', ( #16907, #2000 ), #17034 ) ;
#24270 = ADVANCED_FACE ( 'NONE', ( #10536 ), #12218, .F. ) ;
#24271 = FILL_AREA_STYLE ('',( #10644 ) ) ;
#24272 = EDGE_CURVE ( 'NONE', #15369, #14131, #18142, .T. ) ;
#24273 = LINE ( 'NONE', #4210, #7280 ) ;
#24274 = EDGE_LOOP ( 'NONE', ( #14504, #24104, #25047, #11938 ) ) ;
#24275 = EDGE_LOOP ( 'NONE', ( #8537, #10913, #20727, #22350 ) ) ;
#24276 = ORIENTED_EDGE ( 'NONE', *, *, #13045, .T. ) ;
#24277 = CARTESIAN_POINT ( 'NONE',  ( 17.31606138205699708, 34.87886987267149408, 78.19668729537065133 ) ) ;
#24278 = VECTOR ( 'NONE', #20635, 1000.000000000000000 ) ;
#24279 = CARTESIAN_POINT ( 'NONE',  ( 38.82593461698262871, -4.913682088886101695, 69.62690120949091011 ) ) ;
#24280 = CARTESIAN_POINT ( 'NONE',  ( 40.31606138205700773, 41.44123852234599781, 75.30501292736987295 ) ) ;
#24281 = DIRECTION ( 'NONE',  ( -1.327674326049719602E-15, 0.4425581086832399147, -0.8967398287344627850 ) ) ;
#24282 = VECTOR ( 'NONE', #22655, 1000.000000000000000 ) ;
#24283 = LINE ( 'NONE', #9114, #22554 ) ;
#24284 = ADVANCED_FACE ( 'NONE', ( #11974 ), #18381, .T. ) ;
#24285 = CARTESIAN_POINT ( 'NONE',  ( 43.31606138205700773, -19.13113579875041381, 24.60350147050422720 ) ) ;
#24286 = CARTESIAN_POINT ( 'NONE',  ( 43.31606138205700063, -13.58280000135112964, 20.54174511886706256 ) ) ;
#24287 = CARTESIAN_POINT ( 'NONE',  ( 29.81606138205697576, -4.349482454670887677, -5.142398479549302515 ) ) ;
#24288 = ORIENTED_EDGE ( 'NONE', *, *, #9648, .F. ) ;
#24289 = ORIENTED_EDGE ( 'NONE', *, *, #5667, .F. ) ;
#24290 = CARTESIAN_POINT ( 'NONE',  ( 33.40064408022072939, 41.67000142393845152, 79.57823623207323749 ) ) ;
#24291 = CARTESIAN_POINT ( 'NONE',  ( 39.02088643472237095, -28.91368208888610170, 69.02690120949091579 ) ) ;
#24293 = VECTOR ( 'NONE', #15417, 1000.000000000000000 ) ;
#24292 = CARTESIAN_POINT ( 'NONE',  ( 38.93987200065208754, -24.81368208888610738, 70.42958956619166599 ) ) ;
#24294 = ORIENTED_EDGE ( 'NONE', *, *, #8448, .F. ) ;
#24295 = ORIENTED_EDGE ( 'NONE', *, *, #2321, .F. ) ;
#24296 = DIRECTION ( 'NONE',  ( 1.000000000000000000, 0.000000000000000000, 0.000000000000000000 ) ) ;
#24297 = CARTESIAN_POINT ( 'NONE',  ( 36.87297107704152666, -3.713682088886109511, 72.49904802271743165 ) ) ;
#24298 = CARTESIAN_POINT ( 'NONE',  ( 39.41296390513587511, -1.203840866421910905, 71.08074471024443142 ) ) ;
#24299 = LINE ( 'NONE', #16712, #12057 ) ;
#24300 = CARTESIAN_POINT ( 'NONE',  ( 38.37017380507020192, -8.013682088886108446, 73.71602215082116061 ) ) ;
#24301 = DIRECTION ( 'NONE',  ( 1.000000000000000000, 0.000000000000000000, 0.000000000000000000 ) ) ;
#24302 = CARTESIAN_POINT ( 'NONE',  ( 40.31606138205700773, -7.073990261058225926, 83.13804008194063044 ) ) ;
#24303 = DIRECTION ( 'NONE',  ( 0.000000000000000000, 1.000000000000000000, -1.321694076934710205E-15 ) ) ;
#24304 = FACE_OUTER_BOUND ( 'NONE', #9914, .T. ) ;
#24305 = CARTESIAN_POINT ( 'NONE',  ( 39.20459794252392527, -5.397853031073977625, 82.79825093644204514 ) ) ;
#24306 = EDGE_CURVE ( 'NONE', #8101, #1739, #9560, .T. ) ;
#24307 = VECTOR ( 'NONE', #14251, 1000.000000000000000 ) ;
#24308 = DIRECTION ( 'NONE',  ( 0.000000000000000000, 1.000000000000000000, -4.625929269271481378E-15 ) ) ;
#24309 = ORIENTED_EDGE ( 'NONE', *, *, #25189, .T. ) ;
#24310 = CARTESIAN_POINT ( 'NONE',  ( 39.90994555940143584, -21.47565429014790794, 75.83375200144557482 ) ) ;
#24311 = DIRECTION ( 'NONE',  ( 3.306316923293080268E-47, 1.000000000000000000, -2.999999999999999839E-15 ) ) ;
#24312 = ORIENTED_EDGE ( 'NONE', *, *, #6086, .F. ) ;
#24313 = VERTEX_POINT ( 'NONE', #12349 ) ;
#24314 = CARTESIAN_POINT ( 'NONE',  ( 36.98690846071097127, -15.80384086642191299, 69.45876917294175712 ) ) ;
#24315 = CARTESIAN_POINT ( 'NONE',  ( 36.68196826583682935, -23.61368208888610454, 71.96809898377887293 ) ) ;
#24316 = LINE ( 'NONE', #20859, #22653 ) ;
#24317 = EDGE_CURVE ( 'NONE', #21235, #18110, #3707, .T. ) ;
#24318 = CARTESIAN_POINT ( 'NONE',  ( 38.41621794735363693, -36.60729675983900222, 83.30501292737011454 ) ) ;
#24319 = EDGE_CURVE ( 'NONE', #2496, #20938, #17893, .T. ) ;
#24320 = ORIENTED_EDGE ( 'NONE', *, *, #3014, .T. ) ;
#24321 = DIRECTION ( 'NONE',  ( -1.000000000000000000, 1.115179377413661005E-30, 3.717264591378870232E-16 ) ) ;
#24322 = FACE_OUTER_BOUND ( 'NONE', #3738, .T. ) ;
#24323 = CARTESIAN_POINT ( 'NONE',  ( 40.55423172469004811, -28.41368208888610525, 72.05058123536539938 ) ) ;
#24324 = ORIENTED_EDGE ( 'NONE', *, *, #1598, .T. ) ;
#24325 = VECTOR ( 'NONE', #2409, 1000.000000000000227 ) ;
#24326 = EDGE_CURVE ( 'NONE', #1244, #20311, #2524, .T. ) ;
#24327 = CARTESIAN_POINT ( 'NONE',  ( 33.40064408022072939, 40.95934826813394380, 79.52109337493037344 ) ) ;
#24328 = CYLINDRICAL_SURFACE ( 'NONE', #9166, 2.000000000000001776 ) ;
#24329 = CARTESIAN_POINT ( 'NONE',  ( 39.98359781491296161, 1.586317911113896528, 71.86517103874049894 ) ) ;
#24330 = CARTESIAN_POINT ( 'NONE',  ( 38.31606138205700063, -33.30876147765400219, 71.30501292737024244 ) ) ;
#24331 = AXIS2_PLACEMENT_3D ( 'NONE', #10539, #22246, #12221 ) ;
#24332 = CARTESIAN_POINT ( 'NONE',  ( 39.38009889167650357, -18.21368208888610951, 72.75271321436731853 ) ) ;
#24333 = CARTESIAN_POINT ( 'NONE',  ( 32.81606138205700773, -34.55876147765400219, 75.30501292737011454 ) ) ;
#24334 = EDGE_CURVE ( 'NONE', #12430, #3400, #8250, .T. ) ;
#24335 = CARTESIAN_POINT ( 'NONE',  ( 43.81606138205700063, 36.92314894770294131, 81.17823623207323180 ) ) ;
#24336 = CARTESIAN_POINT ( 'NONE',  ( 38.00113996487112189, -27.70384086642191690, 70.22690120949089021 ) ) ;
#24337 = CARTESIAN_POINT ( 'NONE',  ( 39.75915168707250302, -4.713682088886100630, 70.26145752964252722 ) ) ;
#24338 = CARTESIAN_POINT ( 'NONE',  ( 33.31606138205700773, -13.04008168869995288, 21.66778101221729713 ) ) ;
#24339 = ORIENTED_EDGE ( 'NONE', *, *, #2777, .F. ) ;
#24340 = VECTOR ( 'NONE', #15293, 1000.000000000000000 ) ;
#24341 = CARTESIAN_POINT ( 'NONE',  ( 37.80618814713138676, -7.703840866421907130, 69.62690120949091011 ) ) ;
#24342 = FACE_OUTER_BOUND ( 'NONE', #7339, .T. ) ;
#24343 = VECTOR ( 'NONE', #4711, 1000.000000000000227 ) ;
#24344 = CARTESIAN_POINT ( 'NONE',  ( 37.25202387243752611, -7.213682088886102406, 70.00779233799264034 ) ) ;
#24345 = ORIENTED_EDGE ( 'NONE', *, *, #1650, .T. ) ;
#24346 = CARTESIAN_POINT ( 'NONE',  ( 38.26194895904383486, -17.01368208888610312, 69.04448340153878405 ) ) ;
#24347 = ORIENTED_EDGE ( 'NONE', *, *, #8023, .T. ) ;
#24348 = DIRECTION ( 'NONE',  ( -1.218693434051482139E-16, 0.4425581086832393041, -0.8967398287344630070 ) ) ;
#24349 = CARTESIAN_POINT ( 'NONE',  ( 31.81606138205700418, 39.19123852234599070, 72.05501292736988717 ) ) ;
#24350 = CARTESIAN_POINT ( 'NONE',  ( 37.21915885897815457, -10.20384086642191335, 71.67976084211552745 ) ) ;
#24351 = LINE ( 'NONE', #2715, #20059 ) ;
#24352 = ADVANCED_FACE ( 'NONE', ( #13888 ), #15937, .F. ) ;
#24353 = ORIENTED_EDGE ( 'NONE', *, *, #6264, .T. ) ;
#24354 = CIRCLE ( 'NONE', #5866, 0.7500000000000001110 ) ;
#24355 = LINE ( 'NONE', #16004, #8847 ) ;
#24356 = CARTESIAN_POINT ( 'NONE',  ( 30.81606138205700418, 40.39281886181299797, 84.30501292736984453 ) ) ;
#24357 = CARTESIAN_POINT ( 'NONE',  ( 39.73277004305197124, -15.40384086642191441, 69.52238214136768590 ) ) ;
#24358 = AXIS2_PLACEMENT_3D ( 'NONE', #18400, #988, #5132 ) ;
#24359 = EDGE_CURVE ( 'NONE', #2525, #2891, #19939, .T. ) ;
#24360 = EDGE_CURVE ( 'NONE', #1520, #10123, #8350, .T. ) ;
#24361 = CARTESIAN_POINT ( 'NONE',  ( 40.31606138205700773, -20.22127907754186893, 75.50705395623725735 ) ) ;
#24362 = CARTESIAN_POINT ( 'NONE',  ( 39.95015449827720744, -26.61368208888610809, 70.79240656858104330 ) ) ;
#24363 = DIRECTION ( 'NONE',  ( 0.000000000000000000, 1.000000000000000000, -2.999999999999999839E-15 ) ) ;
#24364 = CARTESIAN_POINT ( 'NONE',  ( 33.81606138205700063, 22.19123852234703520, 80.30501292736994401 ) ) ;
#24365 = CIRCLE ( 'NONE', #20267, 2.000000000000001776 ) ;
#24366 = ORIENTED_EDGE ( 'NONE', *, *, #8668, .F. ) ;
#24367 = LINE ( 'NONE', #12681, #12096 ) ;
#24368 = CARTESIAN_POINT ( 'NONE',  ( 40.31606138205701484, -19.92642959707778516, 24.72592537066031682 ) ) ;
#24369 = VECTOR ( 'NONE', #11911, 1000.000000000000000 ) ;
#24370 = CARTESIAN_POINT ( 'NONE',  ( 39.38009889167648936, -17.40384086642190908, 70.00779233799262613 ) ) ;
#24371 =( NAMED_UNIT ( * ) PLANE_ANGLE_UNIT ( ) SI_UNIT ( $, .RADIAN. ) );
#24372 = PLANE ( 'NONE',  #19471 ) ;
#24373 = DIRECTION ( 'NONE',  ( 0.000000000000000000, 0.8212051873014208914, 0.5706330172266919076 ) ) ;
#24374 = CIRCLE ( 'NONE', #19873, 1.499999999999999778 ) ;
#24375 = FACE_OUTER_BOUND ( 'NONE', #24973, .T. ) ;
#24376 = CARTESIAN_POINT ( 'NONE',  ( 38.37017380507018771, -29.60384086642190837, 69.64448340153876416 ) ) ;
#24377 = CARTESIAN_POINT ( 'NONE',  ( 36.72121174906109786, -21.47450125013314803, 75.83383770706140581 ) ) ;
#24378 = ORIENTED_EDGE ( 'NONE', *, *, #11929, .F. ) ;
#24379 = SHAPE_REPRESENTATION ( 'Pusher Pull Spring', ( #2000 ), #13127 ) ;
#24380 = EDGE_CURVE ( 'NONE', #21638, #9515, #6207, .T. ) ;
#24381 = VECTOR ( 'NONE', #13446, 1000.000000000000000 ) ;
#24382 = CARTESIAN_POINT ( 'NONE',  ( 37.25202387243752611, -23.21368208888610241, 70.00779233799262613 ) ) ;
#24383 = ORIENTED_EDGE ( 'NONE', *, *, #8714, .F. ) ;
#24384 = ORIENTED_EDGE ( 'NONE', *, *, #8300, .F. ) ;
#24385 = DIRECTION ( 'NONE',  ( -1.000000000000000000, 1.301042606982604506E-30, 4.336808689942015271E-16 ) ) ;
#24386 = VECTOR ( 'NONE', #11382, 1000.000000000000000 ) ;
#24387 = DIRECTION ( 'NONE',  ( -1.000000000000000000, 0.000000000000000000, 0.000000000000000000 ) ) ;
#24388 = CARTESIAN_POINT ( 'NONE',  ( 37.21915885897815457, -28.20384086642191335, 71.67976084211551324 ) ) ;
#24389 = CARTESIAN_POINT ( 'NONE',  ( 37.89291511884476904, 0.8863179111139005695, 70.26206559358665515 ) ) ;
#24390 = VERTEX_POINT ( 'NONE', #11037 ) ;
#24391 = ORIENTED_EDGE ( 'NONE', *, *, #20749, .F. ) ;
#24392 = PLANE ( 'NONE',  #5528 ) ;
#24393 = AXIS2_PLACEMENT_3D ( 'NONE', #16349, #2193, #14055 ) ;
#24394 = LINE ( 'NONE', #2749, #12051 ) ;
#24395 = VERTEX_POINT ( 'NONE', #5234 ) ;
#24396 = CARTESIAN_POINT ( 'NONE',  ( 36.68196826583682935, -8.003840866421912281, 70.79240656858108593 ) ) ;
#24397 = DIRECTION ( 'NONE',  ( -1.327674326049719602E-15, 0.4425581086832399147, -0.8967398287344627850 ) ) ;
#24398 = DIRECTION ( 'NONE',  ( -1.000000000000000000, 4.930380657631319405E-32, 1.734723475976804876E-16 ) ) ;
#24399 = ORIENTED_EDGE ( 'NONE', *, *, #6272, .F. ) ;
#24400 = ORIENTED_EDGE ( 'NONE', *, *, #4809, .F. ) ;
#24401 = ORIENTED_EDGE ( 'NONE', *, *, #13023, .T. ) ;
#24402 = DIRECTION ( 'NONE',  ( 0.000000000000000000, 1.000000000000000000, 0.000000000000000000 ) ) ;
#24403 = COLOUR_RGB ( '', 0.08235294, 0.09019608, 0.10196078) ;
#24404 = CARTESIAN_POINT ( 'NONE',  ( 39.95015449827720744, -6.613682088886106314, 70.79240656858107172 ) ) ;
#24405 = EDGE_LOOP ( 'NONE', ( #17349, #16307, #7397, #3517 ) ) ;
#24406 = CARTESIAN_POINT ( 'NONE',  ( 31.81606138205700418, 41.44123852234599070, 73.55501292736987295 ) ) ;
#24407 = AXIS2_PLACEMENT_3D ( 'NONE', #232, #6052, #4123 ) ;
#24408 = DIRECTION ( 'NONE',  ( 1.000000000000000000, 0.000000000000000000, 0.000000000000000000 ) ) ;
#24409 = DIRECTION ( 'NONE',  ( 1.000000000000000000, 0.000000000000000000, 0.000000000000000000 ) ) ;
#24410 = VECTOR ( 'NONE', #15057, 1000.000000000000227 ) ;
#24411 = ADVANCED_FACE ( 'NONE', ( #20568 ), #22496, .F. ) ;
#24412 = DIRECTION ( 'NONE',  ( 0.000000000000000000, 1.000000000000000000, 0.000000000000000000 ) ) ;
#24413 = DIRECTION ( 'NONE',  ( -1.000000000000000000, 0.000000000000000000, 0.000000000000000000 ) ) ;
#24414 = EDGE_CURVE ( 'NONE', #23539, #20035, #1269, .T. ) ;
#24415 = ADVANCED_FACE ( 'NONE', ( #7174 ), #16832, .F. ) ;
#24416 = DIRECTION ( 'NONE',  ( 0.000000000000000000, -0.7516416929448823669, -0.6595716529892345914 ) ) ;
#24417 = VERTEX_POINT ( 'NONE', #10662 ) ;
#24418 = EDGE_LOOP ( 'NONE', ( #11153, #12350, #14077, #16550 ) ) ;
#24419 = DIRECTION ( 'NONE',  ( -1.000000000000000000, 0.000000000000000000, 0.000000000000000000 ) ) ;
#24420 = CARTESIAN_POINT ( 'NONE',  ( 39.12911128074873801, -26.11368208888610809, 73.69843995877326392 ) ) ;
#24421 = PLANE ( 'NONE',  #19301 ) ;
#24422 = CARTESIAN_POINT ( 'NONE',  ( 37.38336156205274818, -15.71368208888609885, 72.12822762946750288 ) ) ;
#24423 = EDGE_LOOP ( 'NONE', ( #21700, #1214, #16088, #17468 ) ) ;
#24424 = ORIENTED_EDGE ( 'NONE', *, *, #20472, .F. ) ;
#24425 = DIRECTION ( 'NONE',  ( 0.000000000000000000, 1.000000000000000000, 0.000000000000000000 ) ) ;
#24426 = CARTESIAN_POINT ( 'NONE',  ( 37.33957961208646736, -3.813682088886109156, 72.81632618279323310 ) ) ;
#24427 = CARTESIAN_POINT ( 'NONE',  ( 38.37017380507018771, -27.60384086642191193, 69.64448340153876416 ) ) ;
#24428 = LINE ( 'NONE', #5251, #2160 ) ;
#24429 = EDGE_CURVE ( 'NONE', #17110, #3839, #22750, .T. ) ;
#24430 = VECTOR ( 'NONE', #25212, 1000.000000000000227 ) ;
#24431 = CARTESIAN_POINT ( 'NONE',  ( 39.12911128074873801, -6.113682088886108978, 73.69843995877330656 ) ) ;
#24432 = CARTESIAN_POINT ( 'NONE',  ( 44.31606138205700063, -20.93319939328399926, 43.78741072286599945 ) ) ;
#24433 = LINE ( 'NONE', #10930, #10833 ) ;
#24434 = PLANE ( 'NONE',  #6892 ) ;
#24435 = DIRECTION ( 'NONE',  ( 0.000000000000000000, 0.8212051873014223347, 0.5706330172266899092 ) ) ;
#24436 = AXIS2_PLACEMENT_3D ( 'NONE', #804, #20274, #4804 ) ;
#24437 = DIRECTION ( 'NONE',  ( -0.1733269559585470521, -3.077057697073492856E-15, -0.9848643390529193686 ) ) ;
#24438 = CARTESIAN_POINT ( 'NONE',  ( 33.31606138205700773, 3.043703737701412226, 64.67489359404071081 ) ) ;
#24439 = AXIS2_PLACEMENT_3D ( 'NONE', #3775, #11530, #9844 ) ;
#24440 = CARTESIAN_POINT ( 'NONE',  ( 41.14099152588522657, -10.60718113818700026, 83.30501292737001506 ) ) ;
#24441 = ORIENTED_EDGE ( 'NONE', *, *, #1948, .F. ) ;
#24442 = CARTESIAN_POINT ( 'NONE',  ( 39.64097644196145609, -21.72505098633521214, 75.31183459773906463 ) ) ;
#24443 = CARTESIAN_POINT ( 'NONE',  ( 40.56606138205695089, 2.967040633637585856, 4.322985289651505525 ) ) ;
#24444 = EDGE_LOOP ( 'NONE', ( #18382, #25183, #14662, #645 ) ) ;
#24445 = EDGE_LOOP ( 'NONE', ( #21113, #9513, #4488, #22465, #10157, #19408, #21710, #13986, #1382, #2264, #21163, #11529, #239, #2222, #9997, #25338 ) ) ;
#24446 = CARTESIAN_POINT ( 'NONE',  ( 40.33642880535521869, -17.30384086642191477, 69.98269868914866265 ) ) ;
#24447 = CARTESIAN_POINT ( 'NONE',  ( 37.33957961208646736, -23.81368208888611093, 72.81632618279320468 ) ) ;
#24448 = DIRECTION ( 'NONE',  ( 0.000000000000000000, 0.6568589528324745297, -0.7540134720837717852 ) ) ;
#24449 = DIRECTION ( 'NONE',  ( 1.000000000000000000, 2.999999999999999839E-15, 0.000000000000000000 ) ) ;
#24450 = ORIENTED_EDGE ( 'NONE', *, *, #17576, .T. ) ;
#24451 = CARTESIAN_POINT ( 'NONE',  ( 44.81606138205700063, 38.19123852234599070, 73.05501292736988717 ) ) ;
#24452 = FACE_OUTER_BOUND ( 'NONE', #21820, .T. ) ;
#24453 = EDGE_CURVE ( 'NONE', #24213, #21678, #13106, .T. ) ;
#24454 = CARTESIAN_POINT ( 'NONE',  ( 40.52078840805428683, -28.61368208888610454, 70.60699637195608602 ) ) ;
#24455 = ORIENTED_EDGE ( 'NONE', *, *, #19038, .T. ) ;
#24456 = CARTESIAN_POINT ( 'NONE',  ( 43.81606138205700063, -37.53049398575952722, 70.06662099985003067 ) ) ;
#24457 = DIRECTION ( 'NONE',  ( -2.048868001712896742E-15, 0.6595716529892345914, -0.7516416929448823669 ) ) ;
#24458 = CARTESIAN_POINT ( 'NONE',  ( 38.37017380507020192, -2.013682088886109334, 73.11602215082118050 ) ) ;
#24459 = LINE ( 'NONE', #20619, #7639 ) ;
#24460 = CARTESIAN_POINT ( 'NONE',  ( 39.98359781491296161, -22.41368208888610525, 71.86517103874047052 ) ) ;
#24461 = LINE ( 'NONE', #892, #24249 ) ;
#24462 = CARTESIAN_POINT ( 'NONE',  ( 40.31606138205700773, -29.30876147765400574, 73.55501292737010033 ) ) ;
#24463 = CARTESIAN_POINT ( 'NONE',  ( 38.26194895904384197, -16.60384086642191193, 72.51602215082118619 ) ) ;
#24464 = CARTESIAN_POINT ( 'NONE',  ( 36.87297107704152666, -3.713682088886109511, 72.49904802271743165 ) ) ;
#24465 = CARTESIAN_POINT ( 'NONE',  ( 34.81606138205687273, 43.19123852234595518, 61.80501292736988006 ) ) ;
#24466 = ORIENTED_EDGE ( 'NONE', *, *, #8306, .F. ) ;
#24467 = CARTESIAN_POINT ( 'NONE',  ( 39.29254315202757653, -6.803840866421915656, 72.81632618279323310 ) ) ;
#24468 = CARTESIAN_POINT ( 'NONE',  ( 40.31606138205702194, -20.80831168696338196, 24.25326155172387033 ) ) ;
#24469 = CARTESIAN_POINT ( 'NONE',  ( 39.98359781491296161, -4.413682088886105248, 71.86517103874048473 ) ) ;
#24470 = VERTEX_POINT ( 'NONE', #7038 ) ;
#24471 = CARTESIAN_POINT ( 'NONE',  ( 38.37017380507020192, -12.01368208888611022, 73.71602215082113219 ) ) ;
#24472 = ORIENTED_EDGE ( 'NONE', *, *, #5700, .F. ) ;
#24473 = LINE ( 'NONE', #24732, #18521 ) ;
#24474 = CARTESIAN_POINT ( 'NONE',  ( 39.41296390513587511, -13.20384086642191157, 71.08074471024441721 ) ) ;
#24475 = ORIENTED_EDGE ( 'NONE', *, *, #6900, .F. ) ;
#24476 = ORIENTED_EDGE ( 'NONE', *, *, #24414, .F. ) ;
#24477 = DIRECTION ( 'NONE',  ( 0.000000000000000000, 0.4425581086832455213, -0.8967398287344598984 ) ) ;
#24478 = DIRECTION ( 'NONE',  ( -1.000000000000000000, -1.000000000000000078E-15, 0.000000000000000000 ) ) ;
#24479 = EDGE_CURVE ( 'NONE', #22728, #7783, #8730, .T. ) ;
#24480 = CARTESIAN_POINT ( 'NONE',  ( 36.36258059203030513, -15.90384086642191264, 69.89063713639259845 ) ) ;
#24481 = CARTESIAN_POINT ( 'NONE',  ( 43.23147868389327897, 41.90149715599300606, 79.87823623207322044 ) ) ;
#24482 = CARTESIAN_POINT ( 'NONE',  ( 39.29254315202756231, -18.81368208888610027, 69.94417936956672577 ) ) ;
#24483 = CARTESIAN_POINT ( 'NONE',  ( 46.91606138205697363, -4.589472609077213328, -6.350807634294790560 ) ) ;
#24484 = DIRECTION ( 'NONE',  ( -1.000000000000000000, 0.000000000000000000, 0.000000000000000000 ) ) ;
#24485 = VERTEX_POINT ( 'NONE', #4851 ) ;
#24486 = CARTESIAN_POINT ( 'NONE',  ( 43.81606138205700063, 38.19123852234599070, 72.05501292736988717 ) ) ;
#24487 = DIRECTION ( 'NONE',  ( -0.1733269559585509378, 0.000000000000000000, -0.9848643390529188135 ) ) ;
#24488 = CARTESIAN_POINT ( 'NONE',  ( 37.33957961208645315, -13.80384086642190766, 69.94417936956672577 ) ) ;
#24489 = DIRECTION ( 'NONE',  ( 1.000000000000000000, 0.000000000000000000, 0.000000000000000000 ) ) ;
#24490 = DIRECTION ( 'NONE',  ( 0.000000000000000000, 0.000000000000000000, 1.000000000000000000 ) ) ;
#24491 = EDGE_CURVE ( 'NONE', #19639, #1958, #10784, .T. ) ;
#24492 = CARTESIAN_POINT ( 'NONE',  ( 38.37017380507020192, -26.01368208888611022, 73.11602215082115208 ) ) ;
#24493 = ADVANCED_FACE ( 'NONE', ( #12845 ), #8862, .F. ) ;
#24494 = LINE ( 'NONE', #12569, #18886 ) ;
#24495 = ADVANCED_FACE ( 'NONE', ( #1236 ), #16700, .F. ) ;
#24496 = DIRECTION ( 'NONE',  ( 1.000000000000000000, 1.734723475976805122E-16, -1.734723475976811039E-16 ) ) ;
#24497 = EDGE_CURVE ( 'NONE', #9366, #13361, #9514, .T. ) ;
#24498 = CARTESIAN_POINT ( 'NONE',  ( 37.80618814713138676, -25.70384086642190979, 69.62690120949091011 ) ) ;
#24499 = ADVANCED_FACE ( 'NONE', ( #3035 ), #10912, .F. ) ;
#24500 = DIRECTION ( 'NONE',  ( 1.734723475976814737E-16, -1.000000000000000000, 3.491481338843135327E-15 ) ) ;
#24501 = ORIENTED_EDGE ( 'NONE', *, *, #2927, .F. ) ;
#24502 = CARTESIAN_POINT ( 'NONE',  ( 37.33957961208646736, -25.81368208888610738, 72.81632618279320468 ) ) ;
#24503 = EDGE_LOOP ( 'NONE', ( #9408, #3642, #20466, #25239 ) ) ;
#24504 = EDGE_LOOP ( 'NONE', ( #8738, #18752, #19443, #16377 ) ) ;
#24505 = CARTESIAN_POINT ( 'NONE',  ( 35.31606138205700773, 7.535758204303438568, 66.26723409915207696 ) ) ;
#24506 = DIRECTION ( 'NONE',  ( -1.000000000000000000, 0.000000000000000000, 0.000000000000000000 ) ) ;
#24507 = CARTESIAN_POINT ( 'NONE',  ( 38.26194895904383486, 0.9863179111139001032, 70.24448340153880110 ) ) ;
#24508 = CARTESIAN_POINT ( 'NONE',  ( 39.51027997493896748, -29.10384086642191193, 71.43714994484031422 ) ) ;
#24509 = VERTEX_POINT ( 'NONE', #14889 ) ;
#24510 = VERTEX_POINT ( 'NONE', #12979 ) ;
#24511 = DIRECTION ( 'NONE',  ( -1.000000000000000000, -3.046345864243081498E-15, -1.366653866685770437E-16 ) ) ;
#24512 = DIRECTION ( 'NONE',  ( -1.734723475976814737E-16, 1.000000000000000000, -3.491481338843135327E-15 ) ) ;
#24513 = VERTEX_POINT ( 'NONE', #20826 ) ;
#24514 = ADVANCED_FACE ( 'NONE', ( #24793, #1362 ), #18510, .T. ) ;
#24515 = SURFACE_STYLE_USAGE ( .BOTH. , #20418 ) ;
#24516 = CARTESIAN_POINT ( 'NONE',  ( 36.68196826583682935, -6.003840866421913169, 70.79240656858108593 ) ) ;
#24517 = EDGE_CURVE ( 'NONE', #20166, #5217, #19022, .T. ) ;
#24518 = CARTESIAN_POINT ( 'NONE',  ( 39.81606138205699352, 8.191238522346989015, 65.30501292736998664 ) ) ;
#24519 = DIRECTION ( 'NONE',  ( -1.000000000000000000, -1.000000000000000078E-15, 0.000000000000000000 ) ) ;
#24520 = VERTEX_POINT ( 'NONE', #22374 ) ;
#24521 = ORIENTED_EDGE ( 'NONE', *, *, #16717, .T. ) ;
#24522 = DIRECTION ( 'NONE',  ( -0.000000000000000000, -3.469446951953613400E-15, -1.000000000000000000 ) ) ;
#24523 = CARTESIAN_POINT ( 'NONE',  ( 37.25202387243752611, -3.213682088886102406, 70.00779233799264034 ) ) ;
#24524 = ADVANCED_FACE ( 'NONE', ( #12604 ), #7559, .T. ) ;
#24525 = CARTESIAN_POINT ( 'NONE',  ( 39.66066260159757917, -29.10876147765399580, 70.75778293607493197 ) ) ;
#24526 = LINE ( 'NONE', #20692, #23144 ) ;
#24527 = CARTESIAN_POINT ( 'NONE',  ( 36.06606138205700063, 5.719301844480432884, 2.701924129460374413 ) ) ;
#24528 = CARTESIAN_POINT ( 'NONE',  ( 31.81606138205700418, 40.39281886181299797, 81.44836866983821722 ) ) ;
#24529 = DIRECTION ( 'NONE',  ( -1.000000000000000000, -1.000000000000000078E-15, 0.000000000000000000 ) ) ;
#24530 = CARTESIAN_POINT ( 'NONE',  ( 40.31606138205700773, -11.51539968388051705, 18.41550321377400934 ) ) ;
#24531 = CARTESIAN_POINT ( 'NONE',  ( 46.81606138205695800, -0.7562224151693112129, -1.633662118351544734 ) ) ;
#24532 = EDGE_LOOP ( 'NONE', ( #16656, #22664, #14639, #12994 ) ) ;
#24533 = EDGE_LOOP ( 'NONE', ( #10889, #12034, #10914, #20929 ) ) ;
#24534 = AXIS2_PLACEMENT_3D ( 'NONE', #13470, #3666, #19521 ) ;
#24535 = DIRECTION ( 'NONE',  ( 0.000000000000000000, -0.5706330172266919076, 0.8212051873014208914 ) ) ;
#24536 = CARTESIAN_POINT ( 'NONE',  ( 45.81606138205700063, 40.39281886181299797, 81.44836866983821722 ) ) ;
#24537 = VECTOR ( 'NONE', #4798, 1000.000000000000000 ) ;
#24538 = AXIS2_PLACEMENT_3D ( 'NONE', #10591, #14572, #2707 ) ;
#24539 = CARTESIAN_POINT ( 'NONE',  ( 38.37017380507020192, -20.01368208888610312, 72.51602215082118619 ) ) ;
#24540 = ORIENTED_EDGE ( 'NONE', *, *, #19347, .F. ) ;
#24541 = VERTEX_POINT ( 'NONE', #9495 ) ;
#24542 = PLANE ( 'NONE',  #19046 ) ;
#24543 = CARTESIAN_POINT ( 'NONE',  ( 36.49096545463212493, 0.4863179111138959954, 71.43714994484035685 ) ) ;
#24544 = CARTESIAN_POINT ( 'NONE',  ( 38.37017380507018771, -21.60384086642190837, 69.64448340153877837 ) ) ;
#24545 = FACE_OUTER_BOUND ( 'NONE', #1038, .T. ) ;
#24546 = CARTESIAN_POINT ( 'NONE',  ( 37.50301148336529167, -9.113682088886102761, 69.06206559358666652 ) ) ;
#24547 = DIRECTION ( 'NONE',  ( 0.000000000000000000, -2.999999999999999839E-15, -1.000000000000000000 ) ) ;
#24548 = DIRECTION ( 'NONE',  ( 1.000000000000000000, 0.000000000000000000, -2.478176394252580155E-16 ) ) ;
#24549 = CARTESIAN_POINT ( 'NONE',  ( 37.31606138205702194, -21.37925193044963024, 31.05911325134166034 ) ) ;
#24550 = AXIS2_PLACEMENT_3D ( 'NONE', #17160, #1546, #17543 ) ;
#24551 = DIRECTION ( 'NONE',  ( 1.734723475976814737E-16, -1.000000000000000000, 3.491481338843135327E-15 ) ) ;
#24552 = CIRCLE ( 'NONE', #5655, 1.500000000000001332 ) ;
#24553 = VECTOR ( 'NONE', #5499, 1000.000000000000227 ) ;
#24554 = CARTESIAN_POINT ( 'NONE',  ( 38.57734783014581836, -5.216337173895527535, 82.80003564993033649 ) ) ;
#24555 = CARTESIAN_POINT ( 'NONE',  ( 33.32114656318253054, -33.12114940777929917, 59.73560686274496589 ) ) ;
#24556 = LINE ( 'NONE', #2802, #14373 ) ;
#24557 = VERTEX_POINT ( 'NONE', #23002 ) ;
#24558 = CARTESIAN_POINT ( 'NONE',  ( 43.31606138205700063, -5.204193249396277032, 83.30501292736992980 ) ) ;
#24559 = DIRECTION ( 'NONE',  ( -6.223655385022149827E-47, 1.000000000000000000, -2.999999999999999839E-15 ) ) ;
#24560 = ORIENTED_EDGE ( 'NONE', *, *, #4304, .T. ) ;
#24561 = ORIENTED_EDGE ( 'NONE', *, *, #4643, .F. ) ;
#24562 = CARTESIAN_POINT ( 'NONE',  ( 39.73277004305197124, -15.40384086642191441, 69.52238214136768590 ) ) ;
#24563 = CARTESIAN_POINT ( 'NONE',  ( 37.25202387243752611, -21.21368208888610241, 70.00779233799262613 ) ) ;
#24564 = LINE ( 'NONE', #18421, #1648 ) ;
#24565 = CIRCLE ( 'NONE', #8138, 1.500000000000001332 ) ;
#24566 =( BOUNDED_CURVE ( )  B_SPLINE_CURVE ( 3, ( #16107, #2317, #23959, #6455 ),
 .UNSPECIFIED., .F., .T. ) 
 B_SPLINE_CURVE_WITH_KNOTS ( ( 4, 4 ),
 ( 0.000000000000000000, 1.570796326794895004 ),
 .UNSPECIFIED. ) 
 CURVE ( )  GEOMETRIC_REPRESENTATION_ITEM ( )  RATIONAL_B_SPLINE_CURVE ( ( 1.000000000000000000, 0.8047378541243649375, 0.8047378541243649375, 1.000000000000000000 ) ) 
 REPRESENTATION_ITEM ( '' )  );
#24567 = CIRCLE ( 'NONE', #4020, 2.499999999999998668 ) ;
#24568 = AXIS2_PLACEMENT_3D ( 'NONE', #11579, #3321, #9271 ) ;
#24569 = DIRECTION ( 'NONE',  ( -2.048868001712896742E-15, 0.6595716529892345914, -0.7516416929448823669 ) ) ;
#24570 = ORIENTED_EDGE ( 'NONE', *, *, #16717, .F. ) ;
#24571 = DIRECTION ( 'NONE',  ( -0.000000000000000000, -1.000000000000000000, 2.848211695852029218E-15 ) ) ;
#24572 = FACE_OUTER_BOUND ( 'NONE', #5665, .T. ) ;
#24573 = CARTESIAN_POINT ( 'NONE',  ( 38.26194895904383486, -25.01368208888610312, 69.04448340153878405 ) ) ;
#24574 = VERTEX_POINT ( 'NONE', #17342 ) ;
#24575 = EDGE_CURVE ( 'NONE', #14052, #24723, #13731, .T. ) ;
#24576 = DIRECTION ( 'NONE',  ( 0.000000000000000000, -0.8967398287344634511, -0.4425581086832385824 ) ) ;
#24577 = APPLICATION_CONTEXT ( 'automotive_design' ) ;
#24579 = EDGE_CURVE ( 'NONE', #13632, #4703, #3429, .T. ) ;
#24578 = DIRECTION ( 'NONE',  ( 0.000000000000000000, 0.000000000000000000, -1.000000000000000000 ) ) ;
#24580 = CARTESIAN_POINT ( 'NONE',  ( 36.68196826583682935, 0.3863179111138967392, 71.96809898377890136 ) ) ;
#24581 = CARTESIAN_POINT ( 'NONE',  ( 47.81606138205695089, -23.19619402982945644, 47.16846523730003327 ) ) ;
#24582 = CARTESIAN_POINT ( 'NONE',  ( 36.68196826583682935, -19.61368208888610809, 71.96809898377888715 ) ) ;
#24583 = CARTESIAN_POINT ( 'NONE',  ( 40.26527270485448184, -20.81370745732132832, 75.90702589141309886 ) ) ;
#24584 = LINE ( 'NONE', #20369, #22785 ) ;
#24585 = CARTESIAN_POINT ( 'NONE',  ( 39.51027997493896748, -21.10384086642191193, 71.43714994484032843 ) ) ;
#24586 = CARTESIAN_POINT ( 'NONE',  ( 36.64852494920107517, -5.413682088886106136, 70.89533451361948835 ) ) ;
#24587 = AXIS2_PLACEMENT_3D ( 'NONE', #14263, #23786, #20186 ) ;
#24588 = ORIENTED_EDGE ( 'NONE', *, *, #1683, .T. ) ;
#24589 = CARTESIAN_POINT ( 'NONE',  ( 31.56606138205707879, -39.99575152356569419, 63.13209164280871022 ) ) ;
#24590 = EDGE_CURVE ( 'NONE', #11508, #9294, #23876, .T. ) ;
#24591 = VERTEX_POINT ( 'NONE', #7296 ) ;
#24592 = CARTESIAN_POINT ( 'NONE',  ( 36.80608444377001831, -2.303840866421914768, 72.40698646996136745 ) ) ;
#24593 = CARTESIAN_POINT ( 'NONE',  ( 43.31606138205700063, -20.88462213363798270, 44.49284693533410717 ) ) ;
#24594 = CARTESIAN_POINT ( 'NONE',  ( 39.82603832034400426, -8.313682088886110932, 72.40698646996135324 ) ) ;
#24595 = ORIENTED_EDGE ( 'NONE', *, *, #24912, .T. ) ;
#24596 = CARTESIAN_POINT ( 'NONE',  ( 40.77203464402485622, -10.51368208888610312, 71.32335560751961623 ) ) ;
#24597 = ORIENTED_EDGE ( 'NONE', *, *, #11646, .T. ) ;
#24598 = DIRECTION ( 'NONE',  ( -1.292986538149619279E-16, 0.9897030922575080769, 0.1431355622335914179 ) ) ;
#24599 = CARTESIAN_POINT ( 'NONE',  ( 37.25260217561390874, -14.00384086642191050, 70.97781676520601479 ) ) ;
#24600 = VECTOR ( 'NONE', #16472, 1000.000000000000000 ) ;
#24601 = CARTESIAN_POINT ( 'NONE',  ( 43.06468080341912241, 3.415100481987967562, 6.350457055188933886 ) ) ;
#24602 = ORIENTED_EDGE ( 'NONE', *, *, #650, .F. ) ;
#24603 = LINE ( 'NONE', #7113, #1431 ) ;
#24604 = DIRECTION ( 'NONE',  ( 0.000000000000000000, -0.8967398287344635621, -0.4425581086832386379 ) ) ;
#24605 = CARTESIAN_POINT ( 'NONE',  ( 36.11133435605973574, -14.00384086642191583, 70.60699637195608602 ) ) ;
#24606 = FACE_OUTER_BOUND ( 'NONE', #17221, .T. ) ;
#24607 = AXIS2_PLACEMENT_3D ( 'NONE', #11264, #18852, #24879 ) ;
#24608 = CARTESIAN_POINT ( 'NONE',  ( 41.06606138205700063, -13.51824891481308910, 37.72654391001022134 ) ) ;
#24609 = CARTESIAN_POINT ( 'NONE',  ( 36.64852494920107517, -17.41368208888610525, 70.89533451361947414 ) ) ;
#24610 = FACE_OUTER_BOUND ( 'NONE', #19135, .T. ) ;
#24611 = CARTESIAN_POINT ( 'NONE',  ( 43.31606138205697221, -3.118133360756952577, 16.65315793475036443 ) ) ;
#24612 = ORIENTED_EDGE ( 'NONE', *, *, #10533, .T. ) ;
#24613 = FACE_OUTER_BOUND ( 'NONE', #97, .T. ) ;
#24614 = CARTESIAN_POINT ( 'NONE',  ( 31.81606138205700418, -31.45856502260510013, 77.07494475056050476 ) ) ;
#24615 = CARTESIAN_POINT ( 'NONE',  ( 37.80618814713138676, -9.703840866421906242, 69.62690120949091011 ) ) ;
#24616 = APPLICATION_PROTOCOL_DEFINITION ( 'draft international standard', 'automotive_design', 1998, #13591 ) ;
#24617 = DIRECTION ( 'NONE',  ( -1.000000000000000000, 5.510910596163088391E-31, 1.836970198721029688E-16 ) ) ;
#24618 = AXIS2_PLACEMENT_3D ( 'NONE', #20982, #16460, #8884 ) ;
#24619 = CARTESIAN_POINT ( 'NONE',  ( 38.82593461698262871, -22.91368208888609459, 69.62690120949091011 ) ) ;
#24620 = CARTESIAN_POINT ( 'NONE',  ( 35.81606138205700063, 37.44123852234599781, 75.30501292736990138 ) ) ;
#24621 = EDGE_CURVE ( 'NONE', #2595, #4447, #9626, .T. ) ;
#24622 = AXIS2_PLACEMENT_3D ( 'NONE', #14676, #22798, #5158 ) ;
#24623 = CARTESIAN_POINT ( 'NONE',  ( 38.82593461698265003, -26.70384086642190624, 73.13360434286902034 ) ) ;
#24624 = LINE ( 'NONE', #10500, #1929 ) ;
#24625 = CIRCLE ( 'NONE', #1195, 0.5000000000000004441 ) ;
#24626 = CARTESIAN_POINT ( 'NONE',  ( 36.49096545463212493, -23.51368208888609601, 71.43714994484030001 ) ) ;
#24627 = ORIENTED_EDGE ( 'NONE', *, *, #21086, .T. ) ;
#24628 = EDGE_LOOP ( 'NONE', ( #5996, #19950, #20450, #16533 ) ) ;
#24629 = LINE ( 'NONE', #3264, #21381 ) ;
#24630 = DIRECTION ( 'NONE',  ( 0.000000000000000000, -0.8212051873014223347, -0.5706330172266899092 ) ) ;
#24631 = CARTESIAN_POINT ( 'NONE',  ( 39.24876120206128860, -0.7136820888861000745, 70.63227792289247020 ) ) ;
#24632 = AXIS2_PLACEMENT_3D ( 'NONE', #4219, #2140, #2396 ) ;
#24633 = CARTESIAN_POINT ( 'NONE',  ( 38.93987200065208754, 1.186317911113898838, 70.42958956619170863 ) ) ;
#24634 = ORIENTED_EDGE ( 'NONE', *, *, #231, .T. ) ;
#24635 = ORIENTED_EDGE ( 'NONE', *, *, #5065, .T. ) ;
#24636 = CARTESIAN_POINT ( 'NONE',  ( 43.81606138205700063, 2.191238522347013440, 73.80501292737000085 ) ) ;
#24637 = CARTESIAN_POINT ( 'NONE',  ( 29.81606138205707879, -39.99575152356569419, 63.13209164280871022 ) ) ;
#24638 = ORIENTED_EDGE ( 'NONE', *, *, #24021, .T. ) ;
#24639 = CARTESIAN_POINT ( 'NONE',  ( 36.31606138205700063, 38.69123852234597649, 69.30501292736988717 ) ) ;
#24640 = CARTESIAN_POINT ( 'NONE',  ( 38.82593461698265003, -6.703840866421914235, 73.13360434286904876 ) ) ;
#24641 = AXIS2_PLACEMENT_3D ( 'NONE', #23787, #21869, #22241 ) ;
#24642 = EDGE_CURVE ( 'NONE', #22382, #22220, #24913, .T. ) ;
#24643 = FACE_OUTER_BOUND ( 'NONE', #17743, .T. ) ;
#24644 = ADVANCED_FACE ( 'NONE', ( #5495 ), #3671, .T. ) ;
#24645 = CARTESIAN_POINT ( 'NONE',  ( 31.91606138205695231, 3.586515973360766996, -0.5067327973472466329 ) ) ;
#24646 = EDGE_CURVE ( 'NONE', #15753, #13887, #8268, .T. ) ;
#24647 = ORIENTED_EDGE ( 'NONE', *, *, #24091, .F. ) ;
#24648 = ORIENTED_EDGE ( 'NONE', *, *, #7926, .T. ) ;
#24649 = ADVANCED_FACE ( 'NONE', ( #19147 ), #9746, .T. ) ;
#24650 = EDGE_CURVE ( 'NONE', #3225, #10140, #23251, .T. ) ;
#24651 = EDGE_LOOP ( 'NONE', ( #24475, #13954, #11190, #20039 ) ) ;
#24652 = VECTOR ( 'NONE', #22654, 1000.000000000000000 ) ;
#24653 = CARTESIAN_POINT ( 'NONE',  ( 36.56606138205700063, 6.004618353093779781, 2.291321535809666354 ) ) ;
#24654 = CARTESIAN_POINT ( 'NONE',  ( 36.49096545463212493, 0.4863179111138961064, 71.43714994484035685 ) ) ;
#24655 = LINE ( 'NONE', #16557, #5674 ) ;
#24656 = DIRECTION ( 'NONE',  ( 0.000000000000000000, 4.914813388431354887E-16, -1.000000000000000000 ) ) ;
#24657 = VECTOR ( 'NONE', #1366, 1000.000000000000000 ) ;
#24658 = ORIENTED_EDGE ( 'NONE', *, *, #24683, .T. ) ;
#24659 = VECTOR ( 'NONE', #8283, 1000.000000000000227 ) ;
#24660 = CARTESIAN_POINT ( 'NONE',  ( 43.31606138205700063, -16.77230293220685198, 77.52306850662458260 ) ) ;
#24661 = EDGE_CURVE ( 'NONE', #1711, #9404, #4974, .T. ) ;
#24662 = CARTESIAN_POINT ( 'NONE',  ( 44.81606138205700063, 35.44123852234597649, 68.80501292736990138 ) ) ;
#24663 = AXIS2_PLACEMENT_3D ( 'NONE', #7871, #5668, #11869 ) ;
#24664 = CARTESIAN_POINT ( 'NONE',  ( 43.81606138205700063, 41.44123852234599070, 73.30501292736985874 ) ) ;
#24665 = DIRECTION ( 'NONE',  ( -1.327674326049719602E-15, 0.4425581086832399147, -0.8967398287344627850 ) ) ;
#24666 =( LENGTH_UNIT ( ) NAMED_UNIT ( * ) SI_UNIT ( .MILLI., .METRE. ) );
#24667 = CIRCLE ( 'NONE', #11950, 1.750000000000001554 ) ;
#24668 = DIRECTION ( 'NONE',  ( 1.000000000000000000, 0.000000000000000000, 0.000000000000000000 ) ) ;
#24669 = ORIENTED_EDGE ( 'NONE', *, *, #15060, .F. ) ;
#24670 = VERTEX_POINT ( 'NONE', #11305 ) ;
#24671 = DIRECTION ( 'NONE',  ( 0.000000000000000000, 3.469446951953613400E-15, 1.000000000000000000 ) ) ;
#24672 = DIRECTION ( 'NONE',  ( 1.000000000000000000, 1.734723475976804876E-16, -1.734723475976814737E-16 ) ) ;
#24673 = CARTESIAN_POINT ( 'NONE',  ( 37.31647492878122563, -17.31368208888610383, 70.72433947564853440 ) ) ;
#24674 = ORIENTED_EDGE ( 'NONE', *, *, #20158, .F. ) ;
#24675 = ORIENTED_EDGE ( 'NONE', *, *, #12866, .T. ) ;
#24676 = LINE ( 'NONE', #10923, #22330 ) ;
#24677 = CARTESIAN_POINT ( 'NONE',  ( 36.68196826583682935, 0.3863179111138967392, 71.96809898377890136 ) ) ;
#24678 = CARTESIAN_POINT ( 'NONE',  ( 36.68196826583682935, -24.00384086642191050, 70.79240656858105751 ) ) ;
#24679 = VECTOR ( 'NONE', #4786, 1000.000000000000000 ) ;
#24680 = DIRECTION ( 'NONE',  ( -1.000000000000000000, 0.000000000000000000, 0.000000000000000000 ) ) ;
#24681 = CARTESIAN_POINT ( 'NONE',  ( 37.61123632939165873, -7.913682088886107913, 73.73360434286902887 ) ) ;
#24682 = VECTOR ( 'NONE', #14796, 1000.000000000000000 ) ;
#24683 = EDGE_CURVE ( 'NONE', #9125, #23772, #27, .T. ) ;
#24684 = LINE ( 'NONE', #2916, #11515 ) ;
#24685 = ADVANCED_FACE ( 'NONE', ( #5871 ), #21083, .T. ) ;
#24686 = LINE ( 'NONE', #10681, #3416 ) ;
#24687 = DIRECTION ( 'NONE',  ( 0.000000000000000000, -1.000000000000000000, 6.938893903907222067E-15 ) ) ;
#24688 = FACE_OUTER_BOUND ( 'NONE', #23892, .T. ) ;
#24689 = CARTESIAN_POINT ( 'NONE',  ( 39.32110845963273960, -5.457236984521631307, 82.79705560817937737 ) ) ;
#24690 = CARTESIAN_POINT ( 'NONE',  ( 38.82593461698264292, 1.296159133578084210, 73.13360434286906298 ) ) ;
#24691 = ADVANCED_FACE ( 'NONE', ( #25038 ), #3545, .F. ) ;
#24692 = CARTESIAN_POINT ( 'NONE',  ( 32.56606138205700773, 45.04446929126255128, 81.37823623207320622 ) ) ;
#24693 = VERTEX_POINT ( 'NONE', #3797 ) ;
#24694 = AXIS2_PLACEMENT_3D ( 'NONE', #23700, #6196, #16097 ) ;
#24695 = DIRECTION ( 'NONE',  ( -1.000000000000000000, -1.734723475976804876E-16, 1.734723475976814737E-16 ) ) ;
#24696 = LINE ( 'NONE', #9013, #24682 ) ;
#24697 = ORIENTED_EDGE ( 'NONE', *, *, #12959, .T. ) ;
#24698 = ORIENTED_EDGE ( 'NONE', *, *, #6928, .F. ) ;
#24699 = UNCERTAINTY_MEASURE_WITH_UNIT (LENGTH_MEASURE( 1.000000000000000082E-05 ), #5109, 'distance_accuracy_value', 'NONE');
#24700 = VECTOR ( 'NONE', #4445, 1000.000000000000114 ) ;
#24701 = CARTESIAN_POINT ( 'NONE',  ( 36.89935272106205133, -20.40384086642192329, 73.23812341099225875 ) ) ;
#24702 = ADVANCED_FACE ( 'NONE', ( #11421 ), #19267, .T. ) ;
#24703 = CARTESIAN_POINT ( 'NONE',  ( 37.69796330110504101, -19.11368208888610098, 69.66206559358661821 ) ) ;
#24704 = DIRECTION ( 'NONE',  ( 0.000000000000000000, 1.000000000000000000, 0.000000000000000000 ) ) ;
#24705 = ORIENTED_EDGE ( 'NONE', *, *, #16991, .F. ) ;
#24706 = DIRECTION ( 'NONE',  ( 0.000000000000000000, 1.000000000000000000, -2.999999999999999839E-15 ) ) ;
#24707 = PLANE ( 'NONE',  #25231 ) ;
#24708 = CARTESIAN_POINT ( 'NONE',  ( 40.55423172469004811, -26.41368208888610880, 72.05058123536539938 ) ) ;
#24709 = VERTEX_POINT ( 'NONE', #1861 ) ;
#24710 = LINE ( 'NONE', #7084, #345 ) ;
#24711 = DIRECTION ( 'NONE',  ( 0.000000000000000000, 0.000000000000000000, 1.000000000000000000 ) ) ;
#24712 = CARTESIAN_POINT ( 'NONE',  ( 39.98359781491296161, -0.4136820888861053591, 71.86517103874048473 ) ) ;
#24713 = CARTESIAN_POINT ( 'NONE',  ( 43.31606138205700773, -18.80550481115970740, 25.27912300651437150 ) ) ;
#24714 = ORIENTED_EDGE ( 'NONE', *, *, #18222, .T. ) ;
#24715 = CARTESIAN_POINT ( 'NONE',  ( 40.14115730948191185, -20.51368208888610312, 71.32335560751960202 ) ) ;
#24716 = VECTOR ( 'NONE', #1998, 1000.000000000000000 ) ;
#24717 = CARTESIAN_POINT ( 'NONE',  ( 40.05426416818898616, -21.26921683217381798, 75.85227166721355729 ) ) ;
#24718 = CARTESIAN_POINT ( 'NONE',  ( 43.81606138205700063, 34.92314894770293421, 79.37823623207323465 ) ) ;
#24719 = CARTESIAN_POINT ( 'NONE',  ( 37.69225076346193504, -17.80384086642191122, 70.42958956619168021 ) ) ;
#24720 = CARTESIAN_POINT ( 'NONE',  ( 36.87297107704152666, -7.713682088886109511, 72.49904802271743165 ) ) ;
#24721 = ORIENTED_EDGE ( 'NONE', *, *, #20895, .F. ) ;
#24722 = CARTESIAN_POINT ( 'NONE',  ( 46.91606138205698073, -6.548589660139384705, -8.069948661059589412 ) ) ;
#24723 = VERTEX_POINT ( 'NONE', #15147 ) ;
#24724 = EDGE_CURVE ( 'NONE', #14165, #8890, #14839, .T. ) ;
#24725 = CARTESIAN_POINT ( 'NONE',  ( 39.98359781491296161, -7.203840866421913347, 70.89533451361947414 ) ) ;
#24726 = CARTESIAN_POINT ( 'NONE',  ( 38.31606138205700063, 42.51966564709218233, 70.30501292737018559 ) ) ;
#24727 = ADVANCED_FACE ( 'NONE', ( #6248, #24124, #9995 ), #4578, .T. ) ;
#24728 = CARTESIAN_POINT ( 'NONE',  ( 37.25260217561390874, -27.61368208888610454, 71.78268878715390144 ) ) ;
#24729 = ORIENTED_EDGE ( 'NONE', *, *, #23865, .F. ) ;
#24730 = CARTESIAN_POINT ( 'NONE',  ( 38.26194895904383486, -11.01368208888609956, 69.04448340153881247 ) ) ;
#24731 = VERTEX_POINT ( 'NONE', #15904 ) ;
#24732 = CARTESIAN_POINT ( 'NONE',  ( 36.31606138205700773, -19.73594837544667513, 24.33996001444790025 ) ) ;
#24733 = CARTESIAN_POINT ( 'NONE',  ( 38.73920764526923932, -9.503840866421912281, 70.26206559358664094 ) ) ;
#24734 = LINE ( 'NONE', #4922, #21712 ) ;
#24735 = ORIENTED_EDGE ( 'NONE', *, *, #23949, .F. ) ;
#24736 = DIRECTION ( 'NONE',  ( 9.925461516413211857E-16, -0.8967398287344600094, -0.4425581086832455213 ) ) ;
#24737 = DIRECTION ( 'NONE',  ( 0.000000000000000000, -1.000000000000000000, 2.775557561562891351E-15 ) ) ;
#24738 = VECTOR ( 'NONE', #3618, 1000.000000000000000 ) ;
#24739 = CARTESIAN_POINT ( 'NONE',  ( 36.07789103942399578, -16.20384086642191690, 72.05058123536544201 ) ) ;
#24740 = CARTESIAN_POINT ( 'NONE',  ( 38.18494427818247061, -22.22127907754186893, 75.30501292736998664 ) ) ;
#24741 = DIRECTION ( 'NONE',  ( 2.690219486203388234E-15, -0.8967398287344627850, -0.4425581086832399147 ) ) ;
#24742 = CARTESIAN_POINT ( 'NONE',  ( 36.80608444377001121, -17.31368208888609672, 70.35351908239857721 ) ) ;
#24743 = FACE_BOUND ( 'NONE', #21563, .T. ) ;
#24744 = EDGE_CURVE ( 'NONE', #23130, #17110, #10752, .T. ) ;
#24745 = LINE ( 'NONE', #22448, #24537 ) ;
#24746 = ORIENTED_EDGE ( 'NONE', *, *, #24479, .T. ) ;
#24747 = DIRECTION ( 'NONE',  ( 1.000000000000000000, 2.168404344971005170E-16, -1.734723475976814737E-16 ) ) ;
#24748 = FACE_OUTER_BOUND ( 'NONE', #2084, .T. ) ;
#24749 = VECTOR ( 'NONE', #17548, 1000.000000000000000 ) ;
#24750 = CARTESIAN_POINT ( 'NONE',  ( 39.38009889167648936, -9.403840866421907307, 70.00779233799264034 ) ) ;
#24751 = DIRECTION ( 'NONE',  ( 0.000000000000000000, 0.000000000000000000, 1.000000000000000000 ) ) ;
#24752 = AXIS2_PLACEMENT_3D ( 'NONE', #6038, #95, #13771 ) ;
#24753 = FACE_OUTER_BOUND ( 'NONE', #21462, .T. ) ;
#24754 = CARTESIAN_POINT ( 'NONE',  ( 38.93415946300897446, -22.11368208888610454, 73.09843995877329803 ) ) ;
#24755 = CARTESIAN_POINT ( 'NONE',  ( 33.40064408022072939, 42.57231754924293909, 79.57823623207323749 ) ) ;
#24756 = VECTOR ( 'NONE', #20959, 1000.000000000000000 ) ;
#24757 = CARTESIAN_POINT ( 'NONE',  ( 38.93415946300896024, -25.50384086642190340, 69.66206559358660400 ) ) ;
#24758 = CARTESIAN_POINT ( 'NONE',  ( 36.80559154321147020, -21.57283688862124649, 75.82675744184658129 ) ) ;
#24759 = CARTESIAN_POINT ( 'NONE',  ( 40.14115730948191185, -22.51368208888609956, 71.32335560751960202 ) ) ;
#24760 = ORIENTED_EDGE ( 'NONE', *, *, #25440, .F. ) ;
#24761 = ORIENTED_EDGE ( 'NONE', *, *, #7513, .F. ) ;
#24762 = FACE_OUTER_BOUND ( 'NONE', #21596, .T. ) ;
#24763 = CARTESIAN_POINT ( 'NONE',  ( 46.91606138205695231, 0.8576245772853769989, -1.570935883000508460 ) ) ;
#24764 = CARTESIAN_POINT ( 'NONE',  ( 37.31647492878122563, -1.313682088886099830, 70.72433947564853440 ) ) ;
#24765 = VERTEX_POINT ( 'NONE', #8062 ) ;
#24766 = ORIENTED_EDGE ( 'NONE', *, *, #13, .T. ) ;
#24767 = LINE ( 'NONE', #1076, #17465 ) ;
#24768 = CARTESIAN_POINT ( 'NONE',  ( 40.31606138205700773, -29.06829118875199924, 75.80501292737000085 ) ) ;
#24769 = VERTEX_POINT ( 'NONE', #21709 ) ;
#24770 = FILL_AREA_STYLE ('',( #3777 ) ) ;
#24771 = CARTESIAN_POINT ( 'NONE',  ( 38.37017380507018771, -5.603840866421908373, 69.64448340153879258 ) ) ;
#24772 = AXIS2_PLACEMENT_3D ( 'NONE', #21759, #1183, #16917 ) ;
#24773 = DIRECTION ( 'NONE',  ( 1.327674326049719602E-15, -0.4425581086832399147, 0.8967398287344627850 ) ) ;
#24774 = EDGE_CURVE ( 'NONE', #12000, #9479, #7032, .T. ) ;
#24775 = CARTESIAN_POINT ( 'NONE',  ( 36.56606138205700063, 5.308699250829721272, 2.416607620847027960 ) ) ;
#24776 = ORIENTED_EDGE ( 'NONE', *, *, #9264, .F. ) ;
#24777 = EDGE_LOOP ( 'NONE', ( #17047, #17318, #13270, #11123 ) ) ;
#24778 = ORIENTED_EDGE ( 'NONE', *, *, #24359, .T. ) ;
#24779 = CARTESIAN_POINT ( 'NONE',  ( 31.81606138205700418, -34.55876147765403061, 66.30501292737011454 ) ) ;
#24780 = CARTESIAN_POINT ( 'NONE',  ( 39.75915168707250302, 1.286317911113898482, 70.26145752964255564 ) ) ;
#24781 = AXIS2_PLACEMENT_3D ( 'NONE', #21001, #2821, #10712 ) ;
#24782 = DIRECTION ( 'NONE',  ( 1.000000000000000000, 0.000000000000000000, 0.000000000000000000 ) ) ;
#24783 = FILL_AREA_STYLE ('',( #16208 ) ) ;
#24784 = DIRECTION ( 'NONE',  ( 2.452751524064188892E-15, -1.000000000000000000, 0.000000000000000000 ) ) ;
#24785 = ORIENTED_EDGE ( 'NONE', *, *, #2194, .T. ) ;
#24786 = DIRECTION ( 'NONE',  ( 0.000000000000000000, 1.000000000000000000, -3.469446951953613794E-15 ) ) ;
#24787 = AXIS2_PLACEMENT_3D ( 'NONE', #11006, #22721, #5210 ) ;
#24788 = PLANE ( 'NONE',  #5060 ) ;
#24789 = AXIS2_PLACEMENT_3D ( 'NONE', #16951, #16694, #24784 ) ;
#24790 = LINE ( 'NONE', #24285, #5349 ) ;
#24791 = CARTESIAN_POINT ( 'NONE',  ( 35.81606138205700063, -6.959910619544162458, 20.07251914782757751 ) ) ;
#24792 = AXIS2_PLACEMENT_3D ( 'NONE', #17321, #21566, #13336 ) ;
#24793 = FACE_BOUND ( 'NONE', #18779, .T. ) ;
#24794 = EDGE_LOOP ( 'NONE', ( #8839, #18050, #22797, #4503 ) ) ;
#24795 = VERTEX_POINT ( 'NONE', #20028 ) ;
#24796 = LINE ( 'NONE', #23005, #12855 ) ;
#24797 = CARTESIAN_POINT ( 'NONE',  ( 41.96606138205694236, 6.105630034208208379, 5.871938670042847974 ) ) ;
#24798 = EDGE_CURVE ( 'NONE', #23124, #5934, #12062, .T. ) ;
#24799 = CARTESIAN_POINT ( 'NONE',  ( 37.38336156205274818, -19.71368208888610596, 72.12822762946750288 ) ) ;
#24800 = ORIENTED_EDGE ( 'NONE', *, *, #11627, .F. ) ;
#24801 = AXIS2_PLACEMENT_3D ( 'NONE', #456, #8083, #10017 ) ;
#24802 = ORIENTED_EDGE ( 'NONE', *, *, #11481, .T. ) ;
#24803 = DIRECTION ( 'NONE',  ( 0.000000000000000000, -0.1918498038142812112, 0.9814242980364923374 ) ) ;
#24804 = ORIENTED_EDGE ( 'NONE', *, *, #11460, .F. ) ;
#24805 = CARTESIAN_POINT ( 'NONE',  ( 37.69796330110504101, -1.113682088886101207, 69.66206559358663242 ) ) ;
#24806 = CARTESIAN_POINT ( 'NONE',  ( 39.82603832034400426, -25.30384086642190766, 70.35351908239857721 ) ) ;
#24807 =( GEOMETRIC_REPRESENTATION_CONTEXT ( 3 ) GLOBAL_UNCERTAINTY_ASSIGNED_CONTEXT ( ( #10814 ) ) GLOBAL_UNIT_ASSIGNED_CONTEXT ( ( #24666, #3426, #17092 ) ) REPRESENTATION_CONTEXT ( 'NONE', 'WORKASPACE' ) );
#24808 = CARTESIAN_POINT ( 'NONE',  ( 47.84183937708599643, -34.55876147765400219, 70.30501292737000085 ) ) ;
#24809 = EDGE_CURVE ( 'NONE', #8986, #7089, #14441, .T. ) ;
#24810 = CARTESIAN_POINT ( 'NONE',  ( 40.77203464402485622, -2.513682088886103116, 71.32335560751961623 ) ) ;
#24811 = AXIS2_PLACEMENT_3D ( 'NONE', #23715, #6210, #6082 ) ;
#24812 = PLANE ( 'NONE',  #19949 ) ;
#24813 = ORIENTED_EDGE ( 'NONE', *, *, #4604, .F. ) ;
#24814 = FACE_OUTER_BOUND ( 'NONE', #7519, .T. ) ;
#24815 = CIRCLE ( 'NONE', #4264, 10.00000000000000000 ) ;
#24816 = CARTESIAN_POINT ( 'NONE',  ( 43.81606138205700063, -33.70281195181703993, 69.07320514641659770 ) ) ;
#24817 = DIRECTION ( 'NONE',  ( 0.000000000000000000, 2.848211695852029218E-15, 1.000000000000000000 ) ) ;
#24818 = FACE_BOUND ( 'NONE', #16138, .T. ) ;
#24819 = CIRCLE ( 'NONE', #4269, 0.2999999999999938827 ) ;
#24820 = CARTESIAN_POINT ( 'NONE',  ( 43.31606138205700063, 7.283211578144648257, 66.04722806671131252 ) ) ;
#24821 = DIRECTION ( 'NONE',  ( 1.000000000000000000, 1.185526135920242153E-16, 8.246758300215675884E-17 ) ) ;
#24822 = EDGE_CURVE ( 'NONE', #10938, #2026, #14238, .T. ) ;
#24823 = EDGE_LOOP ( 'NONE', ( #5009, #2007, #1860, #494, #12333, #19273, #7415, #20733, #5082, #3044, #4240, #12972, #8889, #17795, #15836, #25007, #9046, #24627, #23779 ) ) ;
#24824 = ADVANCED_FACE ( 'NONE', ( #22211 ), #433, .F. ) ;
#24825 = DIRECTION ( 'NONE',  ( -1.000000000000000000, 0.000000000000000000, 0.000000000000000000 ) ) ;
#24826 = CYLINDRICAL_SURFACE ( 'NONE', #16887, 1.750000000000001554 ) ;
#24827 = ORIENTED_EDGE ( 'NONE', *, *, #16616, .T. ) ;
#24828 = EDGE_LOOP ( 'NONE', ( #3651, #22688, #4224, #11237 ) ) ;
#24829 = CARTESIAN_POINT ( 'NONE',  ( 36.11133435605973574, -16.00384086642191406, 70.60699637195608602 ) ) ;
#24830 = ADVANCED_FACE ( 'NONE', ( #13854 ), #19909, .F. ) ;
#24831 = EDGE_CURVE ( 'NONE', #20324, #8796, #11937, .T. ) ;
#24832 = LINE ( 'NONE', #17249, #23930 ) ;
#24833 = CARTESIAN_POINT ( 'NONE',  ( 39.82603832034400426, -18.31368208888610738, 72.40698646996133903 ) ) ;
#24834 = SURFACE_SIDE_STYLE ('',( #20860 ) ) ;
#24835 = ORIENTED_EDGE ( 'NONE', *, *, #12811, .T. ) ;
#24836 = PLANE ( 'NONE',  #17926 ) ;
#24837 = LINE ( 'NONE', #7215, #24410 ) ;
#24838 = EDGE_CURVE ( 'NONE', #17124, #13011, #8315, .T. ) ;
#24839 = CARTESIAN_POINT ( 'NONE',  ( 39.64521430340304420, -24.81368208888610738, 69.45876917294174291 ) ) ;
#24840 = EDGE_CURVE ( 'NONE', #5343, #22990, #561, .T. ) ;
#24841 = VERTEX_POINT ( 'NONE', #23759 ) ;
#24842 = SURFACE_STYLE_USAGE ( .BOTH. , #3208 ) ;
#24843 = LINE ( 'NONE', #22799, #5435 ) ;
#24844 = PRODUCT_DEFINITION_FORMATION_WITH_SPECIFIED_SOURCE ( 'ANY', '', #10148, .NOT_KNOWN. ) ;
#24845 = CARTESIAN_POINT ( 'NONE',  ( 36.87297107704152666, 0.2863179111138939303, 72.49904802271743165 ) ) ;
#24846 = CARTESIAN_POINT ( 'NONE',  ( 44.81606138205700063, -33.00876147765401925, 70.30501292737011454 ) ) ;
#24847 = CARTESIAN_POINT ( 'NONE',  ( 38.82593461698262871, -14.91368208888609992, 69.62690120949091011 ) ) ;
#24848 = CARTESIAN_POINT ( 'NONE',  ( 33.31606138205700773, 2.715274261285174351, 65.05190033008260286 ) ) ;
#24849 = AXIS2_PLACEMENT_3D ( 'NONE', #285, #12555, #6365 ) ;
#24850 = CARTESIAN_POINT ( 'NONE',  ( 33.31606138205700773, -37.81581049437288300, 70.47722359350072452 ) ) ;
#24851 = CARTESIAN_POINT ( 'NONE',  ( 37.25260217561390874, -18.00384086642191050, 70.97781676520601479 ) ) ;
#24852 = CARTESIAN_POINT ( 'NONE',  ( 39.29254315202756231, -2.813682088886101162, 69.94417936956673998 ) ) ;
#24853 = EDGE_LOOP ( 'NONE', ( #15181, #3227, #9223, #3966 ) ) ;
#24854 = CARTESIAN_POINT ( 'NONE',  ( 33.31606138205700773, -12.87480755223283424, 20.78922580900563588 ) ) ;
#24855 = ORIENTED_EDGE ( 'NONE', *, *, #10067, .F. ) ;
#24856 = CARTESIAN_POINT ( 'NONE',  ( 37.25202387243754032, -8.403840866421916189, 72.75271321436733274 ) ) ;
#24857 = DIRECTION ( 'NONE',  ( -0.000000000000000000, 0.5735764363510447161, -0.8191520442889929088 ) ) ;
#24858 = CARTESIAN_POINT ( 'NONE',  ( 37.33957961208646736, -1.813682088886107380, 72.81632618279323310 ) ) ;
#24859 = VERTEX_POINT ( 'NONE', #6125 ) ;
#24860 = CARTESIAN_POINT ( 'NONE',  ( 40.26954217208371034, -6.713682088886101518, 69.89063713639259845 ) ) ;
#24861 = ORIENTED_EDGE ( 'NONE', *, *, #22858, .F. ) ;
#24862 = CARTESIAN_POINT ( 'NONE',  ( 33.31606138205700773, -30.89740888249930961, 1.247106086993583718 ) ) ;
#24863 = CARTESIAN_POINT ( 'NONE',  ( 37.21915885897815457, -8.203840866421909794, 71.67976084211552745 ) ) ;
#24864 = CYLINDRICAL_SURFACE ( 'NONE', #24152, 0.2000000000000057288 ) ;
#24865 = VERTEX_POINT ( 'NONE', #14359 ) ;
#24866 = FACE_OUTER_BOUND ( 'NONE', #19269, .T. ) ;
#24867 = CARTESIAN_POINT ( 'NONE',  ( 38.14273442609844977, 38.69123852234599781, 70.32014858831708182 ) ) ;
#24868 = CARTESIAN_POINT ( 'NONE',  ( 36.36258059203030513, -13.90384086642191264, 69.89063713639259845 ) ) ;
#24869 = CARTESIAN_POINT ( 'NONE',  ( 37.42719827050449055, -22.01767691212489808, 75.30695952225683243 ) ) ;
#24870 = CARTESIAN_POINT ( 'NONE',  ( 39.98359781491296161, -18.41368208888610880, 71.86517103874047052 ) ) ;
#24871 = CARTESIAN_POINT ( 'NONE',  ( 32.81606138205700773, -36.55876147765400930, 73.30501292737011454 ) ) ;
#24872 = DIRECTION ( 'NONE',  ( -1.000000000000000000, 1.115179377413661005E-30, 3.717264591378870232E-16 ) ) ;
#24873 = ADVANCED_FACE ( 'NONE', ( #21836 ), #19141, .T. ) ;
#24874 = ORIENTED_EDGE ( 'NONE', *, *, #13272, .T. ) ;
#24875 = CYLINDRICAL_SURFACE ( 'NONE', #7990, 0.4999999999999982792 ) ;
#24876 = CARTESIAN_POINT ( 'NONE',  ( 39.95015449827720744, -11.00384086642191050, 71.96809898377888715 ) ) ;
#24877 = DIRECTION ( 'NONE',  ( -1.000000000000000000, 0.000000000000000000, 0.000000000000000000 ) ) ;
#24878 = CARTESIAN_POINT ( 'NONE',  ( 38.37017380507020192, -24.01368208888610667, 73.11602215082115208 ) ) ;
#24879 = DIRECTION ( 'NONE',  ( 0.000000000000000000, 1.000000000000000000, 0.000000000000000000 ) ) ;
#24880 = CARTESIAN_POINT ( 'NONE',  ( 39.29254315202757653, -26.80384086642191477, 72.81632618279320468 ) ) ;
#24881 = CARTESIAN_POINT ( 'NONE',  ( 36.80507328770344344, -5.887228176602778973, 83.28319385500074645 ) ) ;
#24882 = CARTESIAN_POINT ( 'NONE',  ( 36.87297107704152666, -17.71368208888610951, 72.49904802271740323 ) ) ;
#24883 = ORIENTED_EDGE ( 'NONE', *, *, #10200, .F. ) ;
#24884 = CARTESIAN_POINT ( 'NONE',  ( 36.36258059203031934, -25.71368208888611306, 72.86986841596734621 ) ) ;
#24885 = ORIENTED_EDGE ( 'NONE', *, *, #11295, .T. ) ;
#24886 = FACE_OUTER_BOUND ( 'NONE', #14352, .T. ) ;
#24887 = CARTESIAN_POINT ( 'NONE',  ( 43.31606138205700063, -37.81581049437287589, 70.47722359350073873 ) ) ;
#24888 = CARTESIAN_POINT ( 'NONE',  ( 39.41296390513587511, -2.413682088886099919, 71.67976084211552745 ) ) ;
#24889 = ORIENTED_EDGE ( 'NONE', *, *, #22949, .T. ) ;
#24890 = VERTEX_POINT ( 'NONE', #9508 ) ;
#24891 = CARTESIAN_POINT ( 'NONE',  ( 32.81606138205700773, 41.44123852234599070, 73.55501292736987295 ) ) ;
#24892 = FACE_OUTER_BOUND ( 'NONE', #10971, .T. ) ;
#24893 = EDGE_LOOP ( 'NONE', ( #5944, #22067, #6069, #20440 ) ) ;
#24894 = CARTESIAN_POINT ( 'NONE',  ( 33.31606138205700773, -22.22127907754180853, 85.30501292736998664 ) ) ;
#24895 = CARTESIAN_POINT ( 'NONE',  ( 39.29254315202757653, -4.803840866421913880, 72.81632618279323310 ) ) ;
#24896 = CARTESIAN_POINT ( 'NONE',  ( 35.56606138205703616, -24.72749677399389157, 32.19456755146972426 ) ) ;
#24897 = PLANE ( 'NONE',  #12641 ) ;
#24898 = ORIENTED_EDGE ( 'NONE', *, *, #1385, .F. ) ;
#24899 = EDGE_CURVE ( 'NONE', #14345, #16500, #19277, .T. ) ;
#24900 = ORIENTED_EDGE ( 'NONE', *, *, #19484, .T. ) ;
#24901 = EDGE_CURVE ( 'NONE', #21826, #13614, #25051, .T. ) ;
#24902 = LINE ( 'NONE', #21195, #7155 ) ;
#24903 = CARTESIAN_POINT ( 'NONE',  ( 37.33957961208646736, 0.1863179111138910105, 72.81632618279323310 ) ) ;
#24904 = CARTESIAN_POINT ( 'NONE',  ( 43.06606138205700063, 42.19123852234601202, 79.18605660143489899 ) ) ;
#24905 = PLANE ( 'NONE',  #22326 ) ;
#24906 = VERTEX_POINT ( 'NONE', #25177 ) ;
#24907 = CARTESIAN_POINT ( 'NONE',  ( 31.91606138205692389, 12.25039015348819582, 8.426307875224583910 ) ) ;
#24908 = DIRECTION ( 'NONE',  ( 0.000000000000000000, -1.000000000000000000, 3.491481338843135327E-15 ) ) ;
#24909 = CARTESIAN_POINT ( 'NONE',  ( 31.56606138205697576, -4.349482454670882348, -5.142398479549302515 ) ) ;
#24910 = ORIENTED_EDGE ( 'NONE', *, *, #7509, .F. ) ;
#24911 = AXIS2_PLACEMENT_3D ( 'NONE', #18558, #17011, #14682 ) ;
#24912 = EDGE_CURVE ( 'NONE', #24670, #19639, #19797, .T. ) ;
#24913 = LINE ( 'NONE', #21589, #13622 ) ;
#24914 = ORIENTED_EDGE ( 'NONE', *, *, #7661, .F. ) ;
#24915 = VERTEX_POINT ( 'NONE', #24923 ) ;
#24916 = DIRECTION ( 'NONE',  ( -1.000000000000000000, 0.000000000000000000, 0.000000000000000000 ) ) ;
#24917 = DIRECTION ( 'NONE',  ( 0.000000000000000000, -1.000000000000000000, 0.000000000000000000 ) ) ;
#24918 = APPLICATION_CONTEXT ( 'automotive_design' ) ;
#24919 = CARTESIAN_POINT ( 'NONE',  ( 39.31564783533280405, -18.31368208888610027, 72.03616607671141026 ) ) ;
#24920 = ORIENTED_EDGE ( 'NONE', *, *, #16792, .F. ) ;
#24921 = VERTEX_POINT ( 'NONE', #19156 ) ;
#24922 = DIRECTION ( 'NONE',  ( -1.734723475976804876E-16, -3.491481338843135327E-15, -1.000000000000000000 ) ) ;
#24923 = CARTESIAN_POINT ( 'NONE',  ( 36.31606138205700063, -12.40281258615396176, 20.95421293576468358 ) ) ;
#24924 = CARTESIAN_POINT ( 'NONE',  ( 37.25202387243754032, -24.40384086642191619, 72.75271321436730432 ) ) ;
#24925 = CARTESIAN_POINT ( 'NONE',  ( 33.63430007298546087, 2.841684771932709186, 6.101742786271089791 ) ) ;
#24926 = CARTESIAN_POINT ( 'NONE',  ( 38.26194895904383486, -3.013682088886100008, 69.04448340153881247 ) ) ;
#24927 = VERTEX_POINT ( 'NONE', #7689 ) ;
#24928 = ORIENTED_EDGE ( 'NONE', *, *, #15865, .F. ) ;
#24929 = LINE ( 'NONE', #19162, #2995 ) ;
#24930 = CARTESIAN_POINT ( 'NONE',  ( 33.56606138205700773, 41.44123852234599781, 75.30501292736988717 ) ) ;
#24931 = FACE_OUTER_BOUND ( 'NONE', #9524, .T. ) ;
#24932 = CARTESIAN_POINT ( 'NONE',  ( 39.20459794252392527, -5.407637742404325820, 83.30316191138764736 ) ) ;
#24933 = CARTESIAN_POINT ( 'NONE',  ( 35.81606138205700063, 41.44123852234599781, 75.30501292736988717 ) ) ;
#24934 = VECTOR ( 'NONE', #10138, 1000.000000000000227 ) ;
#24935 = FACE_OUTER_BOUND ( 'NONE', #14999, .T. ) ;
#24936 = AXIS2_PLACEMENT_3D ( 'NONE', #4685, #12180, #10232 ) ;
#24937 = VECTOR ( 'NONE', #4290, 1000.000000000000000 ) ;
#24938 = ORIENTED_EDGE ( 'NONE', *, *, #13214, .F. ) ;
#24939 = CARTESIAN_POINT ( 'NONE',  ( 40.31606138205700773, 39.69123852234597649, 69.30501292736988717 ) ) ;
#24940 = EDGE_CURVE ( 'NONE', #3119, #5370, #11566, .T. ) ;
#24941 = CARTESIAN_POINT ( 'NONE',  ( 43.31606138205700063, 3.296535697557910538, 65.33616386252352015 ) ) ;
#24942 = VERTEX_POINT ( 'NONE', #7308 ) ;
#24943 = ORIENTED_EDGE ( 'NONE', *, *, #22637, .F. ) ;
#24944 = PRODUCT_DEFINITION_CONTEXT ( 'detailed design', #17889, 'design' ) ;
#24945 = CARTESIAN_POINT ( 'NONE',  ( 35.86008812008917346, -12.10384086642191548, 71.32335560751961623 ) ) ;
#24946 = FACE_OUTER_BOUND ( 'NONE', #5846, .T. ) ;
#24947 = CARTESIAN_POINT ( 'NONE',  ( 36.68196826583682935, -15.61368208888610454, 71.96809898377888715 ) ) ;
#24948 =( NAMED_UNIT ( * ) SI_UNIT ( $, .STERADIAN. ) SOLID_ANGLE_UNIT ( ) );
#24949 = EDGE_LOOP ( 'NONE', ( #13327, #9981, #15084, #12191 ) ) ;
#24950 = CARTESIAN_POINT ( 'NONE',  ( 33.31606138205700773, -19.34822312381090370, 24.15308711316412627 ) ) ;
#24951 = DIRECTION ( 'NONE',  ( -6.505213034913019208E-17, 1.000000000000000000, 0.000000000000000000 ) ) ;
#24952 = CARTESIAN_POINT ( 'NONE',  ( 36.07789103942398867, -23.41368208888610525, 70.70992431699450265 ) ) ;
#24953 = CLOSED_SHELL ( 'NONE', ( #22300, #1504, #8768, #21537, #19546, #10080, #5384, #388, #11019, #18854, #24830, #21077, #13339, #16696, #16487, #4844, #2965, #6399, #3316, #9817, #15064, #15946, #4692, #23948, #7278, #3061, #866, #2667, #24053, #10225, #5766, #20137, #14176, #14156, #13835, #13274, #18375, #21547, #1117, #8252, #15294, #1453, #2488, #2289, #5960, #25413, #25015, #13455, #16823, #15992, #9449, #14116, #19169, #17858, #6914, #22303, #20427, #21076 ) ) ;
#24954 = ORIENTED_EDGE ( 'NONE', *, *, #19017, .T. ) ;
#24955 = EDGE_CURVE ( 'NONE', #11694, #5707, #3345, .T. ) ;
#24956 = CARTESIAN_POINT ( 'NONE',  ( 30.81606138205707524, -38.13418765192407989, 68.51141129791366780 ) ) ;
#24957 = AXIS2_PLACEMENT_3D ( 'NONE', #6337, #19988, #21917 ) ;
#24958 = AXIS2_PLACEMENT_3D ( 'NONE', #12996, #16716, #4998 ) ;
#24959 = CARTESIAN_POINT ( 'NONE',  ( 46.81606138205705747, -33.21365173458013231, 70.96885009038120984 ) ) ;
#24960 = LINE ( 'NONE', #10956, #8478 ) ;
#24961 = EDGE_CURVE ( 'NONE', #19200, #4506, #17761, .T. ) ;
#24962 = EDGE_CURVE ( 'NONE', #58, #13895, #14457, .T. ) ;
#24963 = EDGE_CURVE ( 'NONE', #22626, #1156, #1374, .T. ) ;
#24964 = ADVANCED_FACE ( 'NONE', ( #5624 ), #1740, .T. ) ;
#24965 = CARTESIAN_POINT ( 'NONE',  ( 43.06606138205700063, 42.19123852234599070, 73.55501292736987295 ) ) ;
#24966 = CARTESIAN_POINT ( 'NONE',  ( 38.18531088334250967, -5.204193249396277032, 83.30501292736992980 ) ) ;
#24967 = CARTESIAN_POINT ( 'NONE',  ( 37.69225076346193504, -19.80384086642191477, 70.42958956619168021 ) ) ;
#24968 = CARTESIAN_POINT ( 'NONE',  ( 39.95015449827720744, -0.6136820888861040935, 70.79240656858107172 ) ) ;
#24969 = ORIENTED_EDGE ( 'NONE', *, *, #18469, .F. ) ;
#24970 = LINE ( 'NONE', #24722, #5732 ) ;
#24971 = EDGE_CURVE ( 'NONE', #19274, #18444, #9260, .T. ) ;
#24972 = CARTESIAN_POINT ( 'NONE',  ( 33.31606138205700773, -27.11289203277224402, 56.96090842897168471 ) ) ;
#24973 = EDGE_LOOP ( 'NONE', ( #23563, #10922, #17285, #17703, #1443, #18680, #13233, #6352, #6375, #15793, #22970, #21052, #14518 ) ) ;
#24974 = VECTOR ( 'NONE', #16735, 1000.000000000000000 ) ;
#24975 = ADVANCED_FACE ( 'NONE', ( #3555 ), #11435, .T. ) ;
#24976 = VERTEX_POINT ( 'NONE', #3439 ) ;
#24977 = CARTESIAN_POINT ( 'NONE',  ( 36.80608444377001831, -0.3038408664219130473, 72.40698646996136745 ) ) ;
#24978 = VECTOR ( 'NONE', #14913, 1000.000000000000000 ) ;
#24979 = CARTESIAN_POINT ( 'NONE',  ( 39.24876120206128860, -28.71368208888610241, 70.63227792289242757 ) ) ;
#24980 = CARTESIAN_POINT ( 'NONE',  ( 36.07789103942398867, -11.41368208888610525, 70.70992431699450265 ) ) ;
#24981 = ORIENTED_EDGE ( 'NONE', *, *, #20401, .F. ) ;
#24982 = PLANE ( 'NONE',  #9084 ) ;
#24983 = CARTESIAN_POINT ( 'NONE',  ( 39.37952058850012804, -5.003840866421912281, 71.78268878715392987 ) ) ;
#24984 = CARTESIAN_POINT ( 'NONE',  ( 36.81465384343994884, 41.90149715599300606, 79.87823623207322044 ) ) ;
#24985 = EDGE_CURVE ( 'NONE', #6436, #21126, #21467, .T. ) ;
#24986 = ORIENTED_EDGE ( 'NONE', *, *, #18532, .T. ) ;
#24987 = CARTESIAN_POINT ( 'NONE',  ( 43.81606138205700063, -40.21665604226827639, 68.80894170722476133 ) ) ;
#24988 = CARTESIAN_POINT ( 'NONE',  ( 44.81606138205700063, 41.44123852234599781, 75.30501292736987295 ) ) ;
#24989 = CARTESIAN_POINT ( 'NONE',  ( 40.33642880535521869, -7.303840866421912104, 69.98269868914867686 ) ) ;
#24990 = CARTESIAN_POINT ( 'NONE',  ( 36.80559154321147020, -21.57283688862124649, 75.82675744184658129 ) ) ;
#24991 = CARTESIAN_POINT ( 'NONE',  ( 37.33957961208646736, -19.81368208888611093, 72.81632618279321889 ) ) ;
#24992 = CARTESIAN_POINT ( 'NONE',  ( 44.81606138205700063, -3.831401139557048197, 80.75501292737000369 ) ) ;
#24993 = FACE_OUTER_BOUND ( 'NONE', #6916, .T. ) ;
#24994 = ADVANCED_FACE ( 'NONE', ( #1615 ), #23384, .F. ) ;
#24995 = ORIENTED_EDGE ( 'NONE', *, *, #15077, .T. ) ;
#24996 = AXIS2_PLACEMENT_3D ( 'NONE', #20057, #6410, #18137 ) ;
#24997 = DIRECTION ( 'NONE',  ( 1.734723475976807094E-15, -0.7516416929448819229, -0.6595716529892350355 ) ) ;
#24998 = CARTESIAN_POINT ( 'NONE',  ( 39.29254315202757653, -6.803840866421915656, 72.81632618279323310 ) ) ;
#24999 = APPLICATION_PROTOCOL_DEFINITION ( 'draft international standard', 'automotive_design', 1998, #15728 ) ;
#25000 = CARTESIAN_POINT ( 'NONE',  ( 30.81606138205700418, 40.39281886181299797, 66.30501292737000085 ) ) ;
#25001 = CARTESIAN_POINT ( 'NONE',  ( 38.26194895904383486, -23.01368208888609956, 69.64448340153877837 ) ) ;
#25002 = CARTESIAN_POINT ( 'NONE',  ( 32.81606138205700773, -34.55876147765400930, 73.30501292737011454 ) ) ;
#25003 = AXIS2_PLACEMENT_3D ( 'NONE', #8388, #5979, #19619 ) ;
#25004 = CARTESIAN_POINT ( 'NONE',  ( 36.64852494920107517, -26.20384086642191335, 71.86517103874047052 ) ) ;
#25005 = CARTESIAN_POINT ( 'NONE',  ( 43.81606138205700063, 28.69846577177642288, 66.12638289304319983 ) ) ;
#25006 = CARTESIAN_POINT ( 'NONE',  ( 39.98359781491296161, -20.41368208888610525, 71.86517103874047052 ) ) ;
#25007 = ORIENTED_EDGE ( 'NONE', *, *, #10611, .T. ) ;
#25008 = CARTESIAN_POINT ( 'NONE',  ( 39.12911128074872380, 0.4961591335780889955, 69.06206559358666652 ) ) ;
#25009 = EDGE_LOOP ( 'NONE', ( #6059, #21121, #7404, #25476 ) ) ;
#25010 = CARTESIAN_POINT ( 'NONE',  ( 33.56669025312701393, 3.416671603465565532, 6.349359658337636603 ) ) ;
#25011 = DIRECTION ( 'NONE',  ( -1.000000000000000000, 0.000000000000000000, 0.000000000000000000 ) ) ;
#25012 = CARTESIAN_POINT ( 'NONE',  ( 38.00113996487112189, -27.70384086642191690, 70.22690120949089021 ) ) ;
#25013 = VECTOR ( 'NONE', #20794, 1000.000000000000000 ) ;
#25014 = ORIENTED_EDGE ( 'NONE', *, *, #9198, .F. ) ;
#25015 = ADVANCED_FACE ( 'NONE', ( #9379 ), #3307, .T. ) ;
#25016 = ORIENTED_EDGE ( 'NONE', *, *, #16919, .F. ) ;
#25017 = PLANE ( 'NONE',  #24027 ) ;
#25018 = CARTESIAN_POINT ( 'NONE',  ( 43.77584484464993153, 3.724255437227281362, 6.250601487277855028 ) ) ;
#25019 = ORIENTED_EDGE ( 'NONE', *, *, #17138, .F. ) ;
#25020 = SURFACE_SIDE_STYLE ('',( #21305 ) ) ;
#25021 = CARTESIAN_POINT ( 'NONE',  ( 39.75915168707251723, 1.096159133578084699, 72.49904802271743165 ) ) ;
#25022 = VECTOR ( 'NONE', #20875, 1000.000000000000114 ) ;
#25023 = DIRECTION ( 'NONE',  ( 0.000000000000000000, -1.000000000000000000, 2.999999999999999839E-15 ) ) ;
#25024 = CARTESIAN_POINT ( 'NONE',  ( 33.31606138205700773, -1.963190818658398173, 19.89143565483009013 ) ) ;
#25025 = ORIENTED_EDGE ( 'NONE', *, *, #24054, .F. ) ;
#25026 = AXIS2_PLACEMENT_3D ( 'NONE', #14958, #7233, #19085 ) ;
#25027 = ORIENTED_EDGE ( 'NONE', *, *, #1555, .F. ) ;
#25028 = DIRECTION ( 'NONE',  ( 0.000000000000000000, 0.8212051873014208914, 0.5706330172266919076 ) ) ;
#25029 = CARTESIAN_POINT ( 'NONE',  ( 36.68196826583682935, -3.613682088886103205, 71.96809898377890136 ) ) ;
#25030 = CARTESIAN_POINT ( 'NONE',  ( 36.68196826583682935, -28.00384086642191050, 70.79240656858105751 ) ) ;
#25031 = CARTESIAN_POINT ( 'NONE',  ( 43.31606138205700063, -33.60910547091194900, 60.61426200347987248 ) ) ;
#25032 = VECTOR ( 'NONE', #553, 1000.000000000000000 ) ;
#25033 = CARTESIAN_POINT ( 'NONE',  ( 40.81606138205700773, -6.549308025893449070, 20.35783565644092619 ) ) ;
#25034 = DIRECTION ( 'NONE',  ( 2.122643018205885151E-17, -1.000000000000000000, 3.120611096041553009E-15 ) ) ;
#25035 = CARTESIAN_POINT ( 'NONE',  ( 36.31606138205700773, -21.90577604921434229, 28.73660501626934050 ) ) ;
#25036 = CIRCLE ( 'NONE', #6152, 0.4999999999999982792 ) ;
#25037 = EDGE_LOOP ( 'NONE', ( #315, #4627, #4007, #6790 ) ) ;
#25038 = FACE_OUTER_BOUND ( 'NONE', #2973, .T. ) ;
#25039 = ORIENTED_EDGE ( 'NONE', *, *, #4430, .F. ) ;
#25040 = ORIENTED_EDGE ( 'NONE', *, *, #21995, .F. ) ;
#25042 = ADVANCED_FACE ( 'NONE', ( #23655 ), #3948, .T. ) ;
#25041 = FACE_BOUND ( 'NONE', #16032, .T. ) ;
#25043 = VECTOR ( 'NONE', #8091, 1000.000000000000000 ) ;
#25044 = CARTESIAN_POINT ( 'NONE',  ( 38.00113996487114321, -9.913682088886099919, 72.53360434286905445 ) ) ;
#25045 = EDGE_CURVE ( 'NONE', #3314, #4334, #6137, .T. ) ;
#25046 = CARTESIAN_POINT ( 'NONE',  ( 37.21915885897815457, -11.41368208888610170, 71.08074471024443142 ) ) ;
#25047 = ORIENTED_EDGE ( 'NONE', *, *, #24326, .F. ) ;
#25048 = ADVANCED_FACE ( 'NONE', ( #16045 ), #13865, .F. ) ;
#25049 = ORIENTED_EDGE ( 'NONE', *, *, #839, .F. ) ;
#25050 = FACE_OUTER_BOUND ( 'NONE', #11973, .T. ) ;
#25051 = LINE ( 'NONE', #7820, #5398 ) ;
#25052 = CARTESIAN_POINT ( 'NONE',  ( 36.87297107704149823, -21.90384086642189843, 70.26145752964252722 ) ) ;
#25053 = LINE ( 'NONE', #23387, #9159 ) ;
#25054 = CARTESIAN_POINT ( 'NONE',  ( 37.89291511884476904, -17.11368208888609743, 70.26206559358661252 ) ) ;
#25055 = CIRCLE ( 'NONE', #383, 1.000000000000000888 ) ;
#25056 = ORIENTED_EDGE ( 'NONE', *, *, #18853, .T. ) ;
#25057 = CARTESIAN_POINT ( 'NONE',  ( 38.44711690269065940, -5.204193249396277032, 83.30501292736992980 ) ) ;
#25058 = EDGE_CURVE ( 'NONE', #14856, #23614, #14852, .T. ) ;
#25059 = DIRECTION ( 'NONE',  ( -1.000000000000000000, -1.734723475976814737E-16, 0.000000000000000000 ) ) ;
#25060 = DIRECTION ( 'NONE',  ( 1.734723475976805122E-16, 3.491481338843134933E-15, 1.000000000000000000 ) ) ;
#25061 = AXIS2_PLACEMENT_3D ( 'NONE', #1917, #13913, #3601 ) ;
#25062 = PLANE ( 'NONE',  #16411 ) ;
#25063 = DIRECTION ( 'NONE',  ( 1.000000000000000000, 0.000000000000000000, 0.000000000000000000 ) ) ;
#25064 = AXIS2_PLACEMENT_3D ( 'NONE', #4523, #14435, #16103 ) ;
#25065 = LINE ( 'NONE', #7449, #1210 ) ;
#25066 = EDGE_LOOP ( 'NONE', ( #1304, #25320, #7942, #21356 ) ) ;
#25067 = DIRECTION ( 'NONE',  ( 0.000000000000000000, 2.999999999999999839E-15, 1.000000000000000000 ) ) ;
#25068 = LINE ( 'NONE', #21355, #411 ) ;
#25069 = ORIENTED_EDGE ( 'NONE', *, *, #19399, .T. ) ;
#25070 = VERTEX_POINT ( 'NONE', #12329 ) ;
#25071 = CARTESIAN_POINT ( 'NONE',  ( 40.77203464402485622, -13.10384086642191548, 71.43714994484032843 ) ) ;
#25072 = AXIS2_PLACEMENT_3D ( 'NONE', #14702, #12918, #16637 ) ;
#25073 = DIRECTION ( 'NONE',  ( 0.000000000000000000, 1.000000000000000000, 0.000000000000000000 ) ) ;
#25074 = CARTESIAN_POINT ( 'NONE',  ( 39.98359781491296161, -12.41368208888610525, 71.86517103874047052 ) ) ;
#25075 = VECTOR ( 'NONE', #1534, 1000.000000000000000 ) ;
#25076 =( NAMED_UNIT ( * ) PLANE_ANGLE_UNIT ( ) SI_UNIT ( $, .RADIAN. ) );
#25077 = ORIENTED_EDGE ( 'NONE', *, *, #12906, .T. ) ;
#25078 = CARTESIAN_POINT ( 'NONE',  ( 33.24019963865212191, 3.104051971978903701, 6.135536383744724098 ) ) ;
#25079 = CARTESIAN_POINT ( 'NONE',  ( 36.31606138205701484, -18.91453975041206093, 24.37026150481227305 ) ) ;
#25080 = CARTESIAN_POINT ( 'NONE',  ( 39.12911128074873801, -24.11368208888611164, 73.69843995877326392 ) ) ;
#25081 = AXIS2_PLACEMENT_3D ( 'NONE', #20231, #2693, #6452 ) ;
#25082 = ORIENTED_EDGE ( 'NONE', *, *, #18851, .T. ) ;
#25083 = DIRECTION ( 'NONE',  ( 0.000000000000000000, -1.000000000000000000, 3.469446951953701358E-15 ) ) ;
#25084 = DIRECTION ( 'NONE',  ( 0.000000000000000000, -0.6595716529892415858, 0.7516416929448761497 ) ) ;
#25085 = DIRECTION ( 'NONE',  ( 1.000000000000000000, 2.104045878896135585E-30, -1.734723475976805122E-15 ) ) ;
#25086 = EDGE_CURVE ( 'NONE', #8442, #17440, #7953, .T. ) ;
#25087 = VECTOR ( 'NONE', #14120, 1000.000000000000000 ) ;
#25088 = CARTESIAN_POINT ( 'NONE',  ( 33.31606138205700773, -16.77230293220685198, 77.52306850662458260 ) ) ;
#25089 = CARTESIAN_POINT ( 'NONE',  ( 33.56606138205700773, 42.19123852234595518, 61.30501292736988006 ) ) ;
#25090 = AXIS2_PLACEMENT_3D ( 'NONE', #8757, #22782, #22903 ) ;
#25091 = CARTESIAN_POINT ( 'NONE',  ( 38.26194895904384197, -10.60384086642191370, 72.51602215082118619 ) ) ;
#25092 = CARTESIAN_POINT ( 'NONE',  ( 39.29254315202756231, -0.8136820888860994971, 69.94417936956673998 ) ) ;
#25093 = ORIENTED_EDGE ( 'NONE', *, *, #6282, .F. ) ;
#25094 = DIRECTION ( 'NONE',  ( 0.000000000000000000, 0.5706330172266919076, -0.8212051873014208914 ) ) ;
#25095 = DIRECTION ( 'NONE',  ( 1.000000000000000000, -0.000000000000000000, 0.000000000000000000 ) ) ;
#25096 = ORIENTED_EDGE ( 'NONE', *, *, #9787, .T. ) ;
#25097 = ORIENTED_EDGE ( 'NONE', *, *, #20936, .F. ) ;
#25098 = CARTESIAN_POINT ( 'NONE',  ( 36.49096545463212493, -2.103840866421912814, 71.32335560751963044 ) ) ;
#25099 = EDGE_CURVE ( 'NONE', #1199, #22825, #11820, .T. ) ;
#25100 = ADVANCED_FACE ( 'NONE', ( #19660 ), #319, .T. ) ;
#25101 = CARTESIAN_POINT ( 'NONE',  ( 37.12184278917507640, -27.51368208888609956, 71.43714994484032843 ) ) ;
#25102 = CARTESIAN_POINT ( 'NONE',  ( 36.07789103942398867, -1.413682088886102584, 70.70992431699450265 ) ) ;
#25103 = ORIENTED_EDGE ( 'NONE', *, *, #4361, .T. ) ;
#25104 = FACE_OUTER_BOUND ( 'NONE', #22538, .T. ) ;
#25105 = CARTESIAN_POINT ( 'NONE',  ( 37.25260217561390874, -6.003840866421913169, 70.97781676520604321 ) ) ;
#25106 = EDGE_CURVE ( 'NONE', #21711, #643, #13997, .T. ) ;
#25107 = SURFACE_SIDE_STYLE ('',( #3493 ) ) ;
#25108 = VECTOR ( 'NONE', #8324, 1000.000000000000000 ) ;
#25109 = ORIENTED_EDGE ( 'NONE', *, *, #649, .T. ) ;
#25110 = CARTESIAN_POINT ( 'NONE',  ( 44.81606138205700063, -24.55876147765400574, 72.80501292737008612 ) ) ;
#25111 = DIRECTION ( 'NONE',  ( 1.000000000000000000, 8.911169920151748851E-16, 3.114923731923493702E-16 ) ) ;
#25112 = CARTESIAN_POINT ( 'NONE',  ( 36.89935272106205133, -12.40384086642192152, 73.23812341099225875 ) ) ;
#25113 = AXIS2_PLACEMENT_3D ( 'NONE', #11555, #13607, #25423 ) ;
#25114 = CARTESIAN_POINT ( 'NONE',  ( 43.81606138205700063, 18.19123852234598715, 71.05501292736995822 ) ) ;
#25115 = SURFACE_STYLE_FILL_AREA ( #9699 ) ;
#25116 = CARTESIAN_POINT ( 'NONE',  ( 37.80618814713140097, -15.91368208888610880, 73.13360434286903455 ) ) ;
#25117 = DIRECTION ( 'NONE',  ( 1.000000000000000000, 3.469446951953611033E-15, 0.000000000000000000 ) ) ;
#25118 = ADVANCED_FACE ( 'NONE', ( #69 ), #4078, .F. ) ;
#25119 = CARTESIAN_POINT ( 'NONE',  ( 39.81606138205699352, 8.191238522346989015, 65.30501292736998664 ) ) ;
#25120 = VERTEX_POINT ( 'NONE', #22095 ) ;
#25121 = DIRECTION ( 'NONE',  ( -1.000000000000000000, -2.870367030604242092E-15, 6.397632838472598363E-17 ) ) ;
#25122 = CARTESIAN_POINT ( 'NONE',  ( 38.93415946300897446, -5.503840866421908729, 69.66206559358664663 ) ) ;
#25123 = CONTEXT_DEPENDENT_SHAPE_REPRESENTATION ( #12280, #18173 ) ;
#25124 = CARTESIAN_POINT ( 'NONE',  ( 32.81606138205700773, 3.939299543010435389, 6.271589894995780234 ) ) ;
#25125 = CARTESIAN_POINT ( 'NONE',  ( 38.82593461698262871, -18.91368208888609459, 69.62690120949091011 ) ) ;
#25126 = CYLINDRICAL_SURFACE ( 'NONE', #13530, 0.4999999999999998890 ) ;
#25127 = CARTESIAN_POINT ( 'NONE',  ( 39.98359781491296161, -21.20384086642190979, 70.89533451361945993 ) ) ;
#25128 = EDGE_CURVE ( 'NONE', #6498, #24417, #10342, .T. ) ;
#25129 = CARTESIAN_POINT ( 'NONE',  ( 37.67019652925851148, -5.301893399665129181, 82.80465135712294966 ) ) ;
#25130 = EDGE_CURVE ( 'NONE', #11454, #16162, #15915, .T. ) ;
#25131 = COLOUR_RGB ( '', 0.09019608, 0.27058824, 0.51372549) ;
#25132 = CARTESIAN_POINT ( 'NONE',  ( 37.33957961208646736, -17.81368208888611093, 72.81632618279321889 ) ) ;
#25133 = ORIENTED_EDGE ( 'NONE', *, *, #6905, .T. ) ;
#25134 = CARTESIAN_POINT ( 'NONE',  ( 36.98690846071097837, -21.81368208888610738, 73.30173637941818754 ) ) ;
#25135 = VERTEX_POINT ( 'NONE', #572 ) ;
#25136 = CARTESIAN_POINT ( 'NONE',  ( 30.81606138205700418, -1.357181138186998925, 78.30501292736998664 ) ) ;
#25137 = DIRECTION ( 'NONE',  ( 0.000000000000000000, 0.1771812806364704007, 0.9841782327363373106 ) ) ;
#25138 = CARTESIAN_POINT ( 'NONE',  ( 39.24876120206129571, -22.90384086642191264, 72.12822762946747446 ) ) ;
#25139 = EDGE_CURVE ( 'NONE', #18087, #22306, #10133, .T. ) ;
#25140 = ADVANCED_FACE ( 'NONE', ( #8326 ), #21974, .F. ) ;
#25141 = EDGE_LOOP ( 'NONE', ( #24813, #13716, #18417, #1370 ) ) ;
#25142 = ORIENTED_EDGE ( 'NONE', *, *, #21227, .T. ) ;
#25143 = PLANE ( 'NONE',  #24439 ) ;
#25144 = PLANE ( 'NONE',  #21107 ) ;
#25145 = ORIENTED_EDGE ( 'NONE', *, *, #22647, .T. ) ;
#25146 = CARTESIAN_POINT ( 'NONE',  ( 38.31606138205692247, 12.25039015348821358, 8.426307875224583910 ) ) ;
#25147 = CARTESIAN_POINT ( 'NONE',  ( 36.11133435605973574, -28.00384086642191761, 70.60699637195608602 ) ) ;
#25148 = AXIS2_PLACEMENT_3D ( 'NONE', #3617, #13802, #6 ) ;
#25149 = LINE ( 'NONE', #7663, #8554 ) ;
#25150 = AXIS2_PLACEMENT_3D ( 'NONE', #276, #10477, #21680 ) ;
#25151 = VERTEX_POINT ( 'NONE', #2383 ) ;
#25152 = VERTEX_POINT ( 'NONE', #10257 ) ;
#25153 = CARTESIAN_POINT ( 'NONE',  ( 35.14099152588523367, -10.60718113818700026, 93.30501292736998664 ) ) ;
#25154 = DIRECTION ( 'NONE',  ( 0.000000000000000000, -3.491481338843135327E-15, -1.000000000000000000 ) ) ;
#25155 = VECTOR ( 'NONE', #24045, 1000.000000000000114 ) ;
#25156 = CARTESIAN_POINT ( 'NONE',  ( 36.87297107704151244, -27.90384086642190908, 70.26145752964252722 ) ) ;
#25157 = DIRECTION ( 'NONE',  ( 0.000000000000000000, 0.7540134720837717852, 0.6568589528324746407 ) ) ;
#25158 = VERTEX_POINT ( 'NONE', #18123 ) ;
#25159 = DIRECTION ( 'NONE',  ( 0.000000000000000000, 1.000000000000000000, 0.000000000000000000 ) ) ;
#25160 = EDGE_CURVE ( 'NONE', #13577, #14856, #16166, .T. ) ;
#25161 = DIRECTION ( 'NONE',  ( 1.000000000000000000, 2.751104698760144965E-15, -1.228345504986737969E-16 ) ) ;
#25162 = CARTESIAN_POINT ( 'NONE',  ( 33.31606138205700773, -12.40281258615396531, 20.95421293576468358 ) ) ;
#25163 = CARTESIAN_POINT ( 'NONE',  ( 37.38336156205273397, -5.903840866421909972, 70.63227792289248441 ) ) ;
#25164 = ORIENTED_EDGE ( 'NONE', *, *, #24193, .T. ) ;
#25165 = CARTESIAN_POINT ( 'NONE',  ( 29.81606138205696155, -0.7562224151693598406, -1.633662118351544734 ) ) ;
#25166 = ORIENTED_EDGE ( 'NONE', *, *, #509, .T. ) ;
#25167 = EDGE_LOOP ( 'NONE', ( #8731, #4667 ) ) ;
#25168 = AXIS2_PLACEMENT_3D ( 'NONE', #14911, #5518, #17623 ) ;
#25169 = FACE_OUTER_BOUND ( 'NONE', #18703, .T. ) ;
#25170 = CARTESIAN_POINT ( 'NONE',  ( 37.60469502381300089, -13.21368208888610241, 70.49320253461759478 ) ) ;
#25171 = EDGE_CURVE ( 'NONE', #22094, #14027, #23087, .T. ) ;
#25172 = CARTESIAN_POINT ( 'NONE',  ( 37.31647492878122563, -9.313682088886098498, 70.72433947564853440 ) ) ;
#25173 = EDGE_LOOP ( 'NONE', ( #9376, #10812, #18236, #16795 ) ) ;
#25174 = ORIENTED_EDGE ( 'NONE', *, *, #21926, .F. ) ;
#25175 = CARTESIAN_POINT ( 'NONE',  ( 43.31606138205700063, 7.611641054560886133, 65.67022133066943468 ) ) ;
#25176 = FACE_OUTER_BOUND ( 'NONE', #2642, .T. ) ;
#25177 = CARTESIAN_POINT ( 'NONE',  ( 41.31606138205700063, 3.296535697557906985, 65.33616386252352015 ) ) ;
#25178 = CARTESIAN_POINT ( 'NONE',  ( 37.25202387243754032, -14.40384086642191619, 72.75271321436731853 ) ) ;
#25179 = CARTESIAN_POINT ( 'NONE',  ( 42.85688703463539184, 2.786080299087619228, 6.091846835322635378 ) ) ;
#25180 = AXIS2_PLACEMENT_3D ( 'NONE', #15828, #6045, #19826 ) ;
#25181 = VECTOR ( 'NONE', #2034, 1000.000000000000227 ) ;
#25182 = CARTESIAN_POINT ( 'NONE',  ( 38.63098279924288647, -20.91368208888609814, 70.22690120949090442 ) ) ;
#25183 = ORIENTED_EDGE ( 'NONE', *, *, #3996, .F. ) ;
#25184 = B_SPLINE_CURVE_WITH_KNOTS ( 'NONE', 3,
 ( #14729, #1064, #8827, #12816, #4698, #10879, #14854, #24377, #24758, #11001, #14990, #4812, #5077, #14607, #12943, #22338, #20286, #678 ),
 .UNSPECIFIED., .F., .F.,
 ( 4, 2, 2, 2, 2, 2, 2, 2, 4 ),
 ( 0.000000000000000000, 0.1250000000000000278, 0.2500000000000000555, 0.3749999999999996114, 0.5000000000000007772, 0.6249999999999994449, 0.7499999999999995559, 0.8749999999999998890, 1.000000000000000000 ),
 .UNSPECIFIED. ) ;
#25185 = ORIENTED_EDGE ( 'NONE', *, *, #1683, .F. ) ;
#25186 = CARTESIAN_POINT ( 'NONE',  ( 40.31606138205700773, 38.69123852234597649, 69.30501292736988717 ) ) ;
#25187 = PLANE ( 'NONE',  #15129 ) ;
#25188 = AXIS2_PLACEMENT_3D ( 'NONE', #4184, #22074, #17717 ) ;
#25189 = EDGE_CURVE ( 'NONE', #11454, #4345, #9130, .T. ) ;
#25190 = LINE ( 'NONE', #13627, #14498 ) ;
#25191 = EDGE_CURVE ( 'NONE', #9599, #3377, #20547, .T. ) ;
#25192 = CARTESIAN_POINT ( 'NONE',  ( 40.25357836725066818, -6.691594714027675472, 83.19992197100876297 ) ) ;
#25193 = CARTESIAN_POINT ( 'NONE',  ( 30.81606138205696865, -2.286980848581618986, -4.124514829577853980 ) ) ;
#25194 = PRODUCT_DEFINITION ( 'UNKNOWN', '', #5540, #22906 ) ;
#25195 = CIRCLE ( 'NONE', #12892, 0.5000000000000004441 ) ;
#25196 = CARTESIAN_POINT ( 'NONE',  ( 44.31606138205700063, -20.55619265724211076, 44.11584019928223910 ) ) ;
#25197 = ORIENTED_EDGE ( 'NONE', *, *, #24319, .F. ) ;
#25198 = AXIS2_PLACEMENT_3D ( 'NONE', #8721, #12837, #4596 ) ;
#25199 = DIRECTION ( 'NONE',  ( 0.000000000000000000, -1.000000000000000000, 2.999999999999999839E-15 ) ) ;
#25200 = ORIENTED_EDGE ( 'NONE', *, *, #14747, .F. ) ;
#25201 = EDGE_LOOP ( 'NONE', ( #13923, #23412, #11583, #2747 ) ) ;
#25202 = PRODUCT_DEFINITION_CONTEXT ( 'detailed design', #2543, 'design' ) ;
#25203 = CARTESIAN_POINT ( 'NONE',  ( 36.36258059203030513, -11.90384086642191441, 69.89063713639259845 ) ) ;
#25204 =( BOUNDED_CURVE ( )  B_SPLINE_CURVE ( 3, ( #14331, #23850, #4031, #10098 ),
 .UNSPECIFIED., .F., .T. ) 
 B_SPLINE_CURVE_WITH_KNOTS ( ( 4, 4 ),
 ( 1.794712260653053635E-16, 1.570796326794900333 ),
 .UNSPECIFIED. ) 
 CURVE ( )  GEOMETRIC_REPRESENTATION_ITEM ( )  RATIONAL_B_SPLINE_CURVE ( ( 1.000000000000000000, 0.8047378541243641603, 0.8047378541243641603, 1.000000000000000000 ) ) 
 REPRESENTATION_ITEM ( '' )  );
#25205 = ADVANCED_FACE ( 'NONE', ( #2750 ), #18871, .T. ) ;
#25206 = DIRECTION ( 'NONE',  ( 1.000000000000000000, 1.734723475976805122E-16, 0.000000000000000000 ) ) ;
#25207 = CARTESIAN_POINT ( 'NONE',  ( 38.82593461698262871, -16.91368208888610170, 69.62690120949091011 ) ) ;
#25208 = AXIS2_PLACEMENT_3D ( 'NONE', #20399, #7000, #8561 ) ;
#25209 =( NAMED_UNIT ( * ) PLANE_ANGLE_UNIT ( ) SI_UNIT ( $, .RADIAN. ) );
#25210 = ORIENTED_EDGE ( 'NONE', *, *, #9293, .F. ) ;
#25211 = DIRECTION ( 'NONE',  ( -1.000000000000000000, -1.734723475976799945E-16, 1.734723475976814737E-16 ) ) ;
#25212 = DIRECTION ( 'NONE',  ( -9.999999999999998805E-16, 0.9439899321577399638, 0.3299742535180969494 ) ) ;
#25213 = AXIS2_PLACEMENT_3D ( 'NONE', #24198, #23827, #18052 ) ;
#25214 = CARTESIAN_POINT ( 'NONE',  ( 38.26194895904383486, -21.01368208888610312, 69.04448340153878405 ) ) ;
#25215 = ORIENTED_EDGE ( 'NONE', *, *, #21979, .F. ) ;
#25216 = DIRECTION ( 'NONE',  ( 0.000000000000000000, 1.163336342344340343E-15, -1.000000000000000000 ) ) ;
#25217 = DIRECTION ( 'NONE',  ( 0.000000000000000000, -0.4425581086832400812, 0.8967398287344626739 ) ) ;
#25218 = DIRECTION ( 'NONE',  ( 1.000000000000000000, 1.156482317317870344E-15, 0.000000000000000000 ) ) ;
#25219 = AXIS2_PLACEMENT_3D ( 'NONE', #4046, #23630, #13841 ) ;
#25220 = EDGE_CURVE ( 'NONE', #18567, #17509, #15688, .T. ) ;
#25221 = EDGE_CURVE ( 'NONE', #13157, #18170, #12587, .T. ) ;
#25222 =( GEOMETRIC_REPRESENTATION_CONTEXT ( 3 ) GLOBAL_UNCERTAINTY_ASSIGNED_CONTEXT ( ( #6192 ) ) GLOBAL_UNIT_ASSIGNED_CONTEXT ( ( #10911, #20699, #13101 ) ) REPRESENTATION_CONTEXT ( 'NONE', 'WORKASPACE' ) );
#25223 = CARTESIAN_POINT ( 'NONE',  ( 44.81606138205700063, -21.15876147765410309, 66.30501292737000085 ) ) ;
#25224 = MANIFOLD_SOLID_BREP ( 'NONE', #1116 ) ;
#25225 = CIRCLE ( 'NONE', #20734, 1.750000000000000222 ) ;
#25226 = CARTESIAN_POINT ( 'NONE',  ( 36.99159426505191561, -5.699776791028273948, 83.29373111488995107 ) ) ;
#25227 = CARTESIAN_POINT ( 'NONE',  ( 39.51027997493896748, -15.10384086642191370, 71.43714994484032843 ) ) ;
#25228 = CARTESIAN_POINT ( 'NONE',  ( 38.82593461698262871, 1.086317911113899637, 69.62690120949091011 ) ) ;
#25229 = EDGE_LOOP ( 'NONE', ( #14629, #10100, #279, #22484 ) ) ;
#25230 = CARTESIAN_POINT ( 'NONE',  ( 29.81606138205697931, -5.918777154956199382, -5.916875169744970187 ) ) ;
#25231 = AXIS2_PLACEMENT_3D ( 'NONE', #1140, #12769, #14935 ) ;
#25232 = DIRECTION ( 'NONE',  ( -1.000000000000000000, 0.000000000000000000, 0.000000000000000000 ) ) ;
#25233 = EDGE_LOOP ( 'NONE', ( #2705, #4162, #17442, #1712, #11336 ) ) ;
#25234 = ORIENTED_EDGE ( 'NONE', *, *, #20884, .F. ) ;
#25235 = CARTESIAN_POINT ( 'NONE',  ( 37.25202387243754032, -0.4038408664219159117, 72.75271321436733274 ) ) ;
#25236 = ADVANCED_FACE ( 'NONE', ( #5094 ), #18745, .T. ) ;
#25237 = CARTESIAN_POINT ( 'NONE',  ( 36.68196826583682935, 0.3863179111138967392, 71.96809898377890136 ) ) ;
#25238 = CARTESIAN_POINT ( 'NONE',  ( 36.11133435605973574, -3.613682088886103205, 72.15350918040385864 ) ) ;
#25239 = ORIENTED_EDGE ( 'NONE', *, *, #23401, .T. ) ;
#25240 = DIRECTION ( 'NONE',  ( 1.000000000000000000, 3.083952846180988900E-15, -3.854941057726327830E-16 ) ) ;
#25241 = CARTESIAN_POINT ( 'NONE',  ( 37.89291511884479036, -8.503840866421912281, 72.49843995877331793 ) ) ;
#25242 = STYLED_ITEM ( 'NONE', ( #23932 ), #20587 ) ;
#25243 = CARTESIAN_POINT ( 'NONE',  ( 44.81606138205700063, 1.441238522345979600, 68.80501292737000085 ) ) ;
#25244 = VERTEX_POINT ( 'NONE', #14867 ) ;
#25245 = DIRECTION ( 'NONE',  ( 1.000000000000000000, 0.000000000000000000, 0.000000000000000000 ) ) ;
#25246 = CARTESIAN_POINT ( 'NONE',  ( 36.31606138205700063, 37.44123852234599781, 75.30501292736988717 ) ) ;
#25247 = CARTESIAN_POINT ( 'NONE',  ( 36.07789103942399578, -8.203840866421915123, 72.05058123536544201 ) ) ;
#25248 = CARTESIAN_POINT ( 'NONE',  ( 45.81606138205700063, 34.87886987267150118, 81.44836866983821722 ) ) ;
#25249 =( LENGTH_UNIT ( ) NAMED_UNIT ( * ) SI_UNIT ( .MILLI., .METRE. ) );
#25250 = CARTESIAN_POINT ( 'NONE',  ( 39.95015449827720744, -14.61368208888610454, 70.79240656858105751 ) ) ;
#25251 = DIRECTION ( 'NONE',  ( -1.000000000000000000, -2.699773532888685417E-15, -2.369073068322446951E-15 ) ) ;
#25252 = VECTOR ( 'NONE', #3917, 1000.000000000000114 ) ;
#25253 = DIRECTION ( 'NONE',  ( 0.000000000000000000, 1.000000000000000000, 0.000000000000000000 ) ) ;
#25254 = VERTEX_POINT ( 'NONE', #24639 ) ;
#25255 = LINE ( 'NONE', #3505, #9791 ) ;
#25256 = CARTESIAN_POINT ( 'NONE',  ( 39.95015449827720744, -3.003840866421910505, 71.96809898377888715 ) ) ;
#25257 = SHAPE_DEFINITION_REPRESENTATION ( #6233, #8505 ) ;
#25258 = LINE ( 'NONE', #19224, #15764 ) ;
#25259 = CARTESIAN_POINT ( 'NONE',  ( 39.29254315202756231, -18.81368208888610027, 69.94417936956672577 ) ) ;
#25260 = AXIS2_PLACEMENT_3D ( 'NONE', #16785, #2612, #10749 ) ;
#25261 = LINE ( 'NONE', #5329, #17654 ) ;
#25262 = VECTOR ( 'NONE', #22826, 1000.000000000000000 ) ;
#25263 = CARTESIAN_POINT ( 'NONE',  ( 36.87297107704149823, -15.90384086642190908, 70.26145752964252722 ) ) ;
#25264 = CARTESIAN_POINT ( 'NONE',  ( 37.79523030992096011, -5.268791411979726114, 83.30989578560070186 ) ) ;
#25265 = MANIFOLD_SOLID_BREP ( 'NONE', #20882 ) ;
#25266 = CARTESIAN_POINT ( 'NONE',  ( 39.38009889167650357, -20.21368208888610951, 72.75271321436731853 ) ) ;
#25267 = ORIENTED_EDGE ( 'NONE', *, *, #11687, .F. ) ;
#25268 = CARTESIAN_POINT ( 'NONE',  ( 37.50301148336529167, -21.11368208888610098, 69.06206559358665231 ) ) ;
#25269 = ORIENTED_EDGE ( 'NONE', *, *, #8001, .T. ) ;
#25270 = DIRECTION ( 'NONE',  ( 0.000000000000000000, -0.7540134720837717852, -0.6568589528324746407 ) ) ;
#25271 = VECTOR ( 'NONE', #3501, 1000.000000000000000 ) ;
#25272 = CARTESIAN_POINT ( 'NONE',  ( 38.31606138205700063, -30.30876147765401285, 71.30501292737010033 ) ) ;
#25273 = CARTESIAN_POINT ( 'NONE',  ( 37.69225076346193504, -27.80384086642191477, 70.42958956619166599 ) ) ;
#25274 = ORIENTED_EDGE ( 'NONE', *, *, #2795, .F. ) ;
#25275 = ORIENTED_EDGE ( 'NONE', *, *, #721, .F. ) ;
#25276 = DIRECTION ( 'NONE',  ( 0.000000000000000000, 1.000000000000000000, 0.000000000000000000 ) ) ;
#25277 = FACE_OUTER_BOUND ( 'NONE', #15781, .T. ) ;
#25278 = ORIENTED_EDGE ( 'NONE', *, *, #1528, .T. ) ;
#25279 = PRESENTATION_STYLE_ASSIGNMENT (( #15255 ) ) ;
#25280 = CARTESIAN_POINT ( 'NONE',  ( 39.29254315202757653, 1.196159133578084788, 72.81632618279324731 ) ) ;
#25281 = CARTESIAN_POINT ( 'NONE',  ( 41.81606138205696510, -1.975699482566714904, -4.057200616784870206 ) ) ;
#25282 = DIRECTION ( 'NONE',  ( 0.000000000000000000, 1.000000000000000000, -2.999999999999999839E-15 ) ) ;
#25283 = CIRCLE ( 'NONE', #8865, 1.500000000000000222 ) ;
#25284 = ORIENTED_EDGE ( 'NONE', *, *, #3015, .F. ) ;
#25285 = ADVANCED_FACE ( 'NONE', ( #14622 ), #22477, .T. ) ;
#25286 = EDGE_LOOP ( 'NONE', ( #18328, #18231, #18253, #19148 ) ) ;
#25287 = CARTESIAN_POINT ( 'NONE',  ( 44.81606138205700063, -34.67340937580780036, 71.26505871168839690 ) ) ;
#25288 = EDGE_CURVE ( 'NONE', #12836, #12627, #1841, .T. ) ;
#25289 = CARTESIAN_POINT ( 'NONE',  ( 32.31606138205700063, 10.62769494289597993, 68.29765714199933768 ) ) ;
#25290 = CARTESIAN_POINT ( 'NONE',  ( 39.95015449827720744, -29.00384086642191406, 71.96809898377885872 ) ) ;
#25291 = ADVANCED_FACE ( 'NONE', ( #13212 ), #1706, .T. ) ;
#25292 = FACE_OUTER_BOUND ( 'NONE', #7023, .T. ) ;
#25293 = ADVANCED_FACE ( 'NONE', ( #13337, #11402, #15003 ), #9228, .F. ) ;
#25294 = EDGE_CURVE ( 'NONE', #23130, #8686, #7152, .T. ) ;
#25295 = ORIENTED_EDGE ( 'NONE', *, *, #24233, .F. ) ;
#25296 = DIRECTION ( 'NONE',  ( 0.000000000000000000, 0.7540134720837725624, 0.6568589528324736415 ) ) ;
#25297 = FACE_OUTER_BOUND ( 'NONE', #12375, .T. ) ;
#25298 = DIRECTION ( 'NONE',  ( -1.000000000000000000, -1.187136597504755470E-16, -8.249087426255173666E-17 ) ) ;
#25299 = CARTESIAN_POINT ( 'NONE',  ( 37.89291511884479036, -6.503840866421909617, 72.49843995877331793 ) ) ;
#25300 = ORIENTED_EDGE ( 'NONE', *, *, #25471, .F. ) ;
#25301 = EDGE_CURVE ( 'NONE', #22410, #8119, #17454, .T. ) ;
#25302 = DIRECTION ( 'NONE',  ( -0.000000000000000000, 1.000000000000000000, 0.000000000000000000 ) ) ;
#25303 = VERTEX_POINT ( 'NONE', #15380 ) ;
#25304 = VERTEX_POINT ( 'NONE', #7658 ) ;
#25305 = VECTOR ( 'NONE', #19184, 1000.000000000000000 ) ;
#25306 = ADVANCED_FACE ( 'NONE', ( #19128 ), #1469, .T. ) ;
#25307 = CARTESIAN_POINT ( 'NONE',  ( 40.31606138205701484, -18.91453975041205382, 24.37026150481227305 ) ) ;
#25308 = CARTESIAN_POINT ( 'NONE',  ( 39.41296390513587511, -10.41368208888610170, 71.67976084211552745 ) ) ;
#25309 = CARTESIAN_POINT ( 'NONE',  ( 37.12184278917507640, -11.51368208888610134, 71.43714994484034264 ) ) ;
#25310 = ORIENTED_EDGE ( 'NONE', *, *, #13189, .F. ) ;
#25311 = ORIENTED_EDGE ( 'NONE', *, *, #19973, .F. ) ;
#25312 = LINE ( 'NONE', #13743, #3722 ) ;
#25313 = DIRECTION ( 'NONE',  ( 2.048868001712898319E-15, -0.6595716529892350355, 0.7516416929448821449 ) ) ;
#25314 = ORIENTED_EDGE ( 'NONE', *, *, #12112, .T. ) ;
#25315 = DIRECTION ( 'NONE',  ( 0.000000000000000000, -0.4425581086832400812, 0.8967398287344626739 ) ) ;
#25316 = CARTESIAN_POINT ( 'NONE',  ( 36.49096545463212493, -18.10384086642191193, 71.32335560751961623 ) ) ;
#25317 = DIRECTION ( 'NONE',  ( 1.000000000000000000, 2.999999999999999839E-15, 0.000000000000000000 ) ) ;
#25318 = EDGE_CURVE ( 'NONE', #5267, #5640, #9347, .T. ) ;
#25319 = CARTESIAN_POINT ( 'NONE',  ( 38.37017380507020192, -20.01368208888610312, 72.51602215082118619 ) ) ;
#25320 = ORIENTED_EDGE ( 'NONE', *, *, #3018, .T. ) ;
#25321 = CARTESIAN_POINT ( 'NONE',  ( 39.20459794252392527, -5.407637742404325820, 83.30316191138764736 ) ) ;
#25322 = CARTESIAN_POINT ( 'NONE',  ( 36.80608444377001121, -15.31368208888610027, 70.35351908239860563 ) ) ;
#25323 = DIRECTION ( 'NONE',  ( 1.000000000000000000, 0.000000000000000000, 0.000000000000000000 ) ) ;
#25324 = CARTESIAN_POINT ( 'NONE',  ( 43.81606138205700063, 38.19123852234598360, 71.05501292736988717 ) ) ;
#25325 = CARTESIAN_POINT ( 'NONE',  ( 38.44711690269065940, -5.204193249396277032, 83.30501292736992980 ) ) ;
#25326 = CARTESIAN_POINT ( 'NONE',  ( 36.31606138205700063, 5.691238522346988127, 65.30501292736998664 ) ) ;
#25327 = PRODUCT_DEFINITION_SHAPE ( 'NONE', 'NONE',  #17341 ) ;
#25328 = DIRECTION ( 'NONE',  ( 1.000000000000000000, -0.000000000000000000, 0.000000000000000000 ) ) ;
#25329 = EDGE_LOOP ( 'NONE', ( #6011, #23303, #14360, #8569 ) ) ;
#25330 = DIRECTION ( 'NONE',  ( 0.000000000000000000, -1.000000000000000000, 0.000000000000000000 ) ) ;
#25331 = ORIENTED_EDGE ( 'NONE', *, *, #1555, .T. ) ;
#25332 = EDGE_LOOP ( 'NONE', ( #4760, #18734, #23225, #3326 ) ) ;
#25333 = CARTESIAN_POINT ( 'NONE',  ( 40.55423172469004101, -13.20384086642191690, 70.70992431699450265 ) ) ;
#25334 = ORIENTED_EDGE ( 'NONE', *, *, #19266, .T. ) ;
#25335 = FACE_OUTER_BOUND ( 'NONE', #216, .T. ) ;
#25336 = CARTESIAN_POINT ( 'NONE',  ( 38.37017380507020192, -12.01368208888610845, 73.11602215082116629 ) ) ;
#25337 =( NAMED_UNIT ( * ) PLANE_ANGLE_UNIT ( ) SI_UNIT ( $, .RADIAN. ) );
#25338 = ORIENTED_EDGE ( 'NONE', *, *, #19689, .T. ) ;
#25339 = FACE_OUTER_BOUND ( 'NONE', #5496, .T. ) ;
#25340 = EDGE_CURVE ( 'NONE', #21491, #21773, #17194, .T. ) ;
#25341 = CARTESIAN_POINT ( 'NONE',  ( 43.81606138205700063, 41.44123852234595518, 61.30501292736988006 ) ) ;
#25342 = CARTESIAN_POINT ( 'NONE',  ( 39.73277004305198545, -20.21368208888611306, 73.23812341099225875 ) ) ;
#25343 = ORIENTED_EDGE ( 'NONE', *, *, #8624, .F. ) ;
#25344 = FACE_OUTER_BOUND ( 'NONE', #24532, .T. ) ;
#25345 = LINE ( 'NONE', #1904, #12342 ) ;
#25346 = CARTESIAN_POINT ( 'NONE',  ( 43.81606138205700063, -34.55876147765401640, 70.30501292737011454 ) ) ;
#25347 = CYLINDRICAL_SURFACE ( 'NONE', #11693, 3.999999999999996447 ) ;
#25348 = SURFACE_SIDE_STYLE ('',( #2293 ) ) ;
#25349 = CARTESIAN_POINT ( 'NONE',  ( 36.52316816324354676, 5.898345303533535144, 65.30501292737000085 ) ) ;
#25350 = MANIFOLD_SOLID_BREP ( 'Stock-MAS-155-1', #11424 ) ;
#25351 = CARTESIAN_POINT ( 'NONE',  ( 33.66606138205694521, 5.208890205473720059, 5.429380561359602453 ) ) ;
#25352 = CARTESIAN_POINT ( 'NONE',  ( 37.38336156205273397, -9.903840866421909084, 70.63227792289248441 ) ) ;
#25353 = CARTESIAN_POINT ( 'NONE',  ( 40.14115730948191185, 1.486317911113896884, 71.32335560751963044 ) ) ;
#25354 = ORIENTED_EDGE ( 'NONE', *, *, #15631, .T. ) ;
#25355 = CARTESIAN_POINT ( 'NONE',  ( 44.31606138205700063, 10.29926546647973851, 68.67466387804121553 ) ) ;
#25356 = DIRECTION ( 'NONE',  ( 2.776799322558808202E-15, -0.8967398287344627850, -0.4425581086832400257 ) ) ;
#25357 = ORIENTED_EDGE ( 'NONE', *, *, #5242, .T. ) ;
#25358 = VERTEX_POINT ( 'NONE', #5467 ) ;
#25359 = CARTESIAN_POINT ( 'NONE',  ( 39.75915168707251723, 1.096159133578084699, 72.49904802271743165 ) ) ;
#25360 = CARTESIAN_POINT ( 'NONE',  ( 39.24876120206128860, -26.71368208888610596, 70.63227792289242757 ) ) ;
#25361 = CARTESIAN_POINT ( 'NONE',  ( 37.61123632939165873, -3.913682088886108357, 73.73360434286902887 ) ) ;
#25362 = EDGE_LOOP ( 'NONE', ( #19835, #17732, #20309, #21463 ) ) ;
#25363 = CARTESIAN_POINT ( 'NONE',  ( 44.81606138205700063, 41.44123852234599781, 74.30501292736987295 ) ) ;
#25364 = ADVANCED_FACE ( 'NONE', ( #11660 ), #1340, .F. ) ;
#25365 = CARTESIAN_POINT ( 'NONE',  ( 37.38336156205273397, -5.903840866421909972, 70.63227792289248441 ) ) ;
#25366 = EDGE_CURVE ( 'NONE', #11694, #10306, #13525, .T. ) ;
#25367 = AXIS2_PLACEMENT_3D ( 'NONE', #5319, #9574, #23325 ) ;
#25368 = AXIS2_PLACEMENT_3D ( 'NONE', #17856, #5998, #13852 ) ;
#25369 = FACE_OUTER_BOUND ( 'NONE', #22742, .T. ) ;
#25370 = ORIENTED_EDGE ( 'NONE', *, *, #2372, .T. ) ;
#25371 = DIRECTION ( 'NONE',  ( 0.000000000000000000, 1.000000000000000000, 0.000000000000000000 ) ) ;
#25372 = EDGE_CURVE ( 'NONE', #126, #9062, #13452, .T. ) ;
#25373 = CARTESIAN_POINT ( 'NONE',  ( 43.31606138205700063, 7.282926244446933595, 65.60596383066929604 ) ) ;
#25374 = CARTESIAN_POINT ( 'NONE',  ( 39.64521430340305841, -12.80384086642191832, 73.30173637941818754 ) ) ;
#25375 = LINE ( 'NONE', #21538, #15209 ) ;
#25376 = CARTESIAN_POINT ( 'NONE',  ( 36.87297107704152666, -13.71368208888610773, 72.49904802271740323 ) ) ;
#25377 = CARTESIAN_POINT ( 'NONE',  ( 33.97785981918843845, 3.164009542231369654, 6.379277577875881455 ) ) ;
#25378 = CARTESIAN_POINT ( 'NONE',  ( 40.31606138205702194, -20.48251210171515879, 31.50167136002490764 ) ) ;
#25379 = DIRECTION ( 'NONE',  ( -2.545659196538654441E-15, 0.8967398287344627850, 0.4425581086832399147 ) ) ;
#25380 = CARTESIAN_POINT ( 'NONE',  ( 40.14115730948191185, -3.103840866421910150, 71.43714994484034264 ) ) ;
#25381 = AXIS2_PLACEMENT_3D ( 'NONE', #18963, #12793, #9188 ) ;
#25382 = CONTEXT_DEPENDENT_SHAPE_REPRESENTATION ( #4715, #22064 ) ;
#25383 = CARTESIAN_POINT ( 'NONE',  ( 33.42374909935192306, 3.629904212211158221, 6.320127632620215152 ) ) ;
#25384 = CARTESIAN_POINT ( 'NONE',  ( 39.98359781491296161, -18.41368208888610880, 71.86517103874047052 ) ) ;
#25385 = TOROIDAL_SURFACE ( 'NONE', #10593, 0.2314957320545545372, 0.5000000000000000000 ) ;
#25386 = VECTOR ( 'NONE', #19527, 1000.000000000000227 ) ;
#25387 = CYLINDRICAL_SURFACE ( 'NONE', #25465, 1.500000000000001332 ) ;
#25388 = CARTESIAN_POINT ( 'NONE',  ( 39.98359781491296161, -15.20384086642191157, 70.89533451361945993 ) ) ;
#25389 = FACE_OUTER_BOUND ( 'NONE', #7229, .T. ) ;
#25390 = CARTESIAN_POINT ( 'NONE',  ( 39.29254315202756231, -16.81368208888610383, 69.94417936956672577 ) ) ;
#25391 = ORIENTED_EDGE ( 'NONE', *, *, #19638, .T. ) ;
#25392 = CARTESIAN_POINT ( 'NONE',  ( 36.11133435605973574, -19.61368208888610454, 72.15350918040385864 ) ) ;
#25393 = VERTEX_POINT ( 'NONE', #20097 ) ;
#25394 = CYLINDRICAL_SURFACE ( 'NONE', #24252, 3.999999999999999556 ) ;
#25395 = LINE ( 'NONE', #21426, #5894 ) ;
#25396 = CARTESIAN_POINT ( 'NONE',  ( 39.02742774030101458, -25.40384086642191264, 70.49320253461758057 ) ) ;
#25397 = ORIENTED_EDGE ( 'NONE', *, *, #17615, .T. ) ;
#25398 = VERTEX_POINT ( 'NONE', #23621 ) ;
#25399 = DIRECTION ( 'NONE',  ( 0.000000000000000000, 1.000000000000000000, 0.000000000000000000 ) ) ;
#25400 = DIRECTION ( 'NONE',  ( -8.758115402030106693E-47, 1.000000000000000000, -3.469446951953613400E-15 ) ) ;
#25401 = ORIENTED_EDGE ( 'NONE', *, *, #15385, .F. ) ;
#25402 = CARTESIAN_POINT ( 'NONE',  ( 38.82593461698265003, -0.7038408664219141242, 73.13360434286904876 ) ) ;
#25403 = AXIS2_PLACEMENT_3D ( 'NONE', #22030, #17928, #24076 ) ;
#25404 = VECTOR ( 'NONE', #20784, 1000.000000000000000 ) ;
#25405 = VECTOR ( 'NONE', #833, 1000.000000000000114 ) ;
#25406 = LINE ( 'NONE', #5981, #25252 ) ;
#25407 = CARTESIAN_POINT ( 'NONE',  ( 40.55423172469004811, -0.4136820888861054146, 72.05058123536544201 ) ) ;
#25408 = DIRECTION ( 'NONE',  ( 1.000000000000000000, 0.000000000000000000, 0.000000000000000000 ) ) ;
#25409 = EDGE_LOOP ( 'NONE', ( #90, #17901, #24158, #10542 ) ) ;
#25410 = ORIENTED_EDGE ( 'NONE', *, *, #12594, .F. ) ;
#25411 = FACE_OUTER_BOUND ( 'NONE', #11390, .T. ) ;
#25412 = PLANE ( 'NONE',  #12236 ) ;
#25413 = ADVANCED_FACE ( 'NONE', ( #9722 ), #16346, .T. ) ;
#25414 = CARTESIAN_POINT ( 'NONE',  ( 39.29254315202757653, -18.80384086642191477, 72.81632618279321889 ) ) ;
#25415 = CARTESIAN_POINT ( 'NONE',  ( 36.31606138205700063, 38.69123852234599070, 73.55501292736988717 ) ) ;
#25416 = VERTEX_POINT ( 'NONE', #24195 ) ;
#25417 = PLANE ( 'NONE',  #7376 ) ;
#25418 = DIRECTION ( 'NONE',  ( 0.000000000000000000, -1.000000000000000000, 2.999999999999999839E-15 ) ) ;
#25419 = DIRECTION ( 'NONE',  ( 0.000000000000000000, -2.999999999999999839E-15, -1.000000000000000000 ) ) ;
#25420 = CARTESIAN_POINT ( 'NONE',  ( 37.21915885897815457, -8.203840866421909794, 71.67976084211552745 ) ) ;
#25421 = ORIENTED_EDGE ( 'NONE', *, *, #3442, .T. ) ;
#25422 = VECTOR ( 'NONE', #21106, 1000.000000000000227 ) ;
#25423 = DIRECTION ( 'NONE',  ( 1.000000000000000000, 6.938893903907222067E-15, 0.000000000000000000 ) ) ;
#25424 = VERTEX_POINT ( 'NONE', #15634 ) ;
#25425 = ORIENTED_EDGE ( 'NONE', *, *, #20592, .F. ) ;
#25426 = DIRECTION ( 'NONE',  ( 0.000000000000000000, -2.913263826201159484E-15, -1.000000000000000000 ) ) ;
#25427 = AXIS2_PLACEMENT_3D ( 'NONE', #16204, #15949, #6303 ) ;
#25428 = CARTESIAN_POINT ( 'NONE',  ( 39.37952058850012804, -10.61368208888610276, 70.97781676520601479 ) ) ;
#25429 = EDGE_CURVE ( 'NONE', #10938, #12466, #10649, .T. ) ;
#25430 = CIRCLE ( 'NONE', #10251, 0.9999999999999937828 ) ;
#25431 = EDGE_CURVE ( 'NONE', #4753, #15622, #6536, .T. ) ;
#25432 = CARTESIAN_POINT ( 'NONE',  ( 37.89291511884476904, -13.11368208888610454, 70.26206559358661252 ) ) ;
#25433 = EDGE_LOOP ( 'NONE', ( #11532, #9480, #6849, #14775 ) ) ;
#25434 = ORIENTED_EDGE ( 'NONE', *, *, #18706, .T. ) ;
#25435 = LINE ( 'NONE', #16041, #11992 ) ;
#25436 = LINE ( 'NONE', #67, #10404 ) ;
#25437 = EDGE_LOOP ( 'NONE', ( #7680, #10510, #2462, #18497 ) ) ;
#25438 = DIRECTION ( 'NONE',  ( -1.000000000000000000, -2.168404344971005170E-16, 1.734723475976814737E-16 ) ) ;
#25439 = CARTESIAN_POINT ( 'NONE',  ( 37.80618814713138676, -19.70384086642190624, 69.62690120949091011 ) ) ;
#25440 = EDGE_CURVE ( 'NONE', #9628, #14366, #6690, .T. ) ;
#25441 = VECTOR ( 'NONE', #9603, 1000.000000000000000 ) ;
#25442 = EDGE_CURVE ( 'NONE', #11430, #6274, #19279, .T. ) ;
#25443 = DIRECTION ( 'NONE',  ( -2.312964634635742267E-15, 0.8967398287344626739, 0.4425581086832399147 ) ) ;
#25444 = MANIFOLD_SOLID_BREP ( 'NONE', #18818 ) ;
#25445 = CYLINDRICAL_SURFACE ( 'NONE', #19928, 1.099999999999999867 ) ;
#25446 = CARTESIAN_POINT ( 'NONE',  ( 37.69225076346193504, -19.81368208888610383, 72.33091598616826445 ) ) ;
#25447 = VECTOR ( 'NONE', #5025, 1000.000000000000000 ) ;
#25448 = ORIENTED_EDGE ( 'NONE', *, *, #2982, .T. ) ;
#25449 = VECTOR ( 'NONE', #22205, 1000.000000000000000 ) ;
#25450 = CARTESIAN_POINT ( 'NONE',  ( 36.31606138205700773, -22.71854986786759412, 31.51329497139233737 ) ) ;
#25451 = CARTESIAN_POINT ( 'NONE',  ( 37.69796330110504101, -13.11368208888609921, 69.66206559358663242 ) ) ;
#25452 = EDGE_CURVE ( 'NONE', #21232, #20277, #18425, .T. ) ;
#25453 = CARTESIAN_POINT ( 'NONE',  ( 46.81606138205705037, -30.46100403034031245, 72.05704881431053366 ) ) ;
#25454 = DIRECTION ( 'NONE',  ( 0.000000000000000000, 0.7540134720837717852, 0.6568589528324746407 ) ) ;
#25455 = VECTOR ( 'NONE', #5140, 1000.000000000000000 ) ;
#25456 = FACE_BOUND ( 'NONE', #14608, .T. ) ;
#25457 = FACE_OUTER_BOUND ( 'NONE', #7207, .T. ) ;
#25458 = CIRCLE ( 'NONE', #14771, 3.000000000000000444 ) ;
#25459 = DIRECTION ( 'NONE',  ( -1.000000000000000000, 0.000000000000000000, 0.000000000000000000 ) ) ;
#25460 = VERTEX_POINT ( 'NONE', #14304 ) ;
#25461 = LINE ( 'NONE', #9396, #16467 ) ;
#25462 = ORIENTED_EDGE ( 'NONE', *, *, #15098, .T. ) ;
#25463 = EDGE_LOOP ( 'NONE', ( #4888, #19161 ) ) ;
#25464 = CARTESIAN_POINT ( 'NONE',  ( 38.26194895904384197, -12.60384086642191903, 73.71602215082113219 ) ) ;
#25465 = AXIS2_PLACEMENT_3D ( 'NONE', #8028, #1947, #21799 ) ;
#25466 = ORIENTED_EDGE ( 'NONE', *, *, #5481, .T. ) ;
#25467 = CARTESIAN_POINT ( 'NONE',  ( 30.81606138205697221, -29.47337283097074234, 44.07055847651731995 ) ) ;
#25468 = CARTESIAN_POINT ( 'NONE',  ( 39.75915168707250302, -14.71368208888610063, 70.26145752964251301 ) ) ;
#25469 = EDGE_CURVE ( 'NONE', #21232, #12198, #18177, .T. ) ;
#25470 = AXIS2_PLACEMENT_3D ( 'NONE', #3851, #11348, #25217 ) ;
#25471 = EDGE_CURVE ( 'NONE', #18988, #22382, #5703, .T. ) ;
#25472 = EDGE_LOOP ( 'NONE', ( #11793, #11364 ) ) ;
#25473 = CARTESIAN_POINT ( 'NONE',  ( 36.31606138205703616, -24.57005561077093247, 31.87555009596680478 ) ) ;
#25474 = DIRECTION ( 'NONE',  ( 0.000000000000000000, -1.000000000000000000, 2.999999999999999839E-15 ) ) ;
#25475 = CARTESIAN_POINT ( 'NONE',  ( 40.33642880535524000, -14.31368208888610738, 72.77780686321126780 ) ) ;
#25476 = ORIENTED_EDGE ( 'NONE', *, *, #6030, .F. ) ;
#25477 = VECTOR ( 'NONE', #4977, 1000.000000000000000 ) ;
#25478 =( LENGTH_UNIT ( ) NAMED_UNIT ( * ) SI_UNIT ( .MILLI., .METRE. ) );
#25479 = CARTESIAN_POINT ( 'NONE',  ( 35.81606138205700063, 37.44123852234599781, 74.30501292736988717 ) ) ;
#25480 = EDGE_CURVE ( 'NONE', #4935, #17850, #11788, .T. ) ;
#25481 = CIRCLE ( 'NONE', #9494, 1.500000000000001332 ) ;
#25482 = CARTESIAN_POINT ( 'NONE',  ( 31.81606138205700418, -30.95005513552129983, 81.04249030099066431 ) ) ;
#25483 = VECTOR ( 'NONE', #19836, 1000.000000000000000 ) ;
#25484 = DIRECTION ( 'NONE',  ( 0.000000000000000000, 0.8191520442889929088, 0.5735764363510447161 ) ) ;
#25485 = CARTESIAN_POINT ( 'NONE',  ( 43.06468080341912241, 3.415100481987967562, 6.350457055188933886 ) ) ;
#25486 = VECTOR ( 'NONE', #18639, 1000.000000000000114 ) ;
#25487 = CARTESIAN_POINT ( 'NONE',  ( 37.60469502381300799, -14.40384086642191441, 72.26730301774234988 ) ) ;
#25488 = CARTESIAN_POINT ( 'NONE',  ( 37.69225076346193504, 0.1961591335780874246, 70.42958956619168021 ) ) ;
#25489 = NEXT_ASSEMBLY_USAGE_OCCURRENCE ( 'NAUO1', ' ', ' ', #8861, #11212, $ ) ;
#25490 = NEXT_ASSEMBLY_USAGE_OCCURRENCE ( 'NAUO2', ' ', ' ', #8861, #17663, $ ) ;
#25491 = NEXT_ASSEMBLY_USAGE_OCCURRENCE ( 'NAUO3', ' ', ' ', #8861, #3162, $ ) ;
#25492 = NEXT_ASSEMBLY_USAGE_OCCURRENCE ( 'NAUO4', ' ', ' ', #8861, #17341, $ ) ;
#25493 = NEXT_ASSEMBLY_USAGE_OCCURRENCE ( 'NAUO5', ' ', ' ', #8861, #10107, $ ) ;
#25494 = NEXT_ASSEMBLY_USAGE_OCCURRENCE ( 'NAUO6', ' ', ' ', #8861, #9653, $ ) ;
#25495 = NEXT_ASSEMBLY_USAGE_OCCURRENCE ( 'NAUO7', ' ', ' ', #8861, #23307, $ ) ;
#25496 = NEXT_ASSEMBLY_USAGE_OCCURRENCE ( 'NAUO8', ' ', ' ', #8861, #20652, $ ) ;
#25497 = NEXT_ASSEMBLY_USAGE_OCCURRENCE ( 'NAUO9', ' ', ' ', #8861, #25194, $ ) ;
#25498 = NEXT_ASSEMBLY_USAGE_OCCURRENCE ( 'NAUO10', ' ', ' ', #8861, #2830, $ ) ;
#25499 = NEXT_ASSEMBLY_USAGE_OCCURRENCE ( 'NAUO11', ' ', ' ', #8861, #23001, $ ) ;
#25500 = NEXT_ASSEMBLY_USAGE_OCCURRENCE ( 'NAUO12', ' ', ' ', #8861, #21901, $ ) ;
#25501 = NEXT_ASSEMBLY_USAGE_OCCURRENCE ( 'NAUO13', ' ', ' ', #8861, #19220, $ ) ;
ENDSEC;
END-ISO-10303-21;
